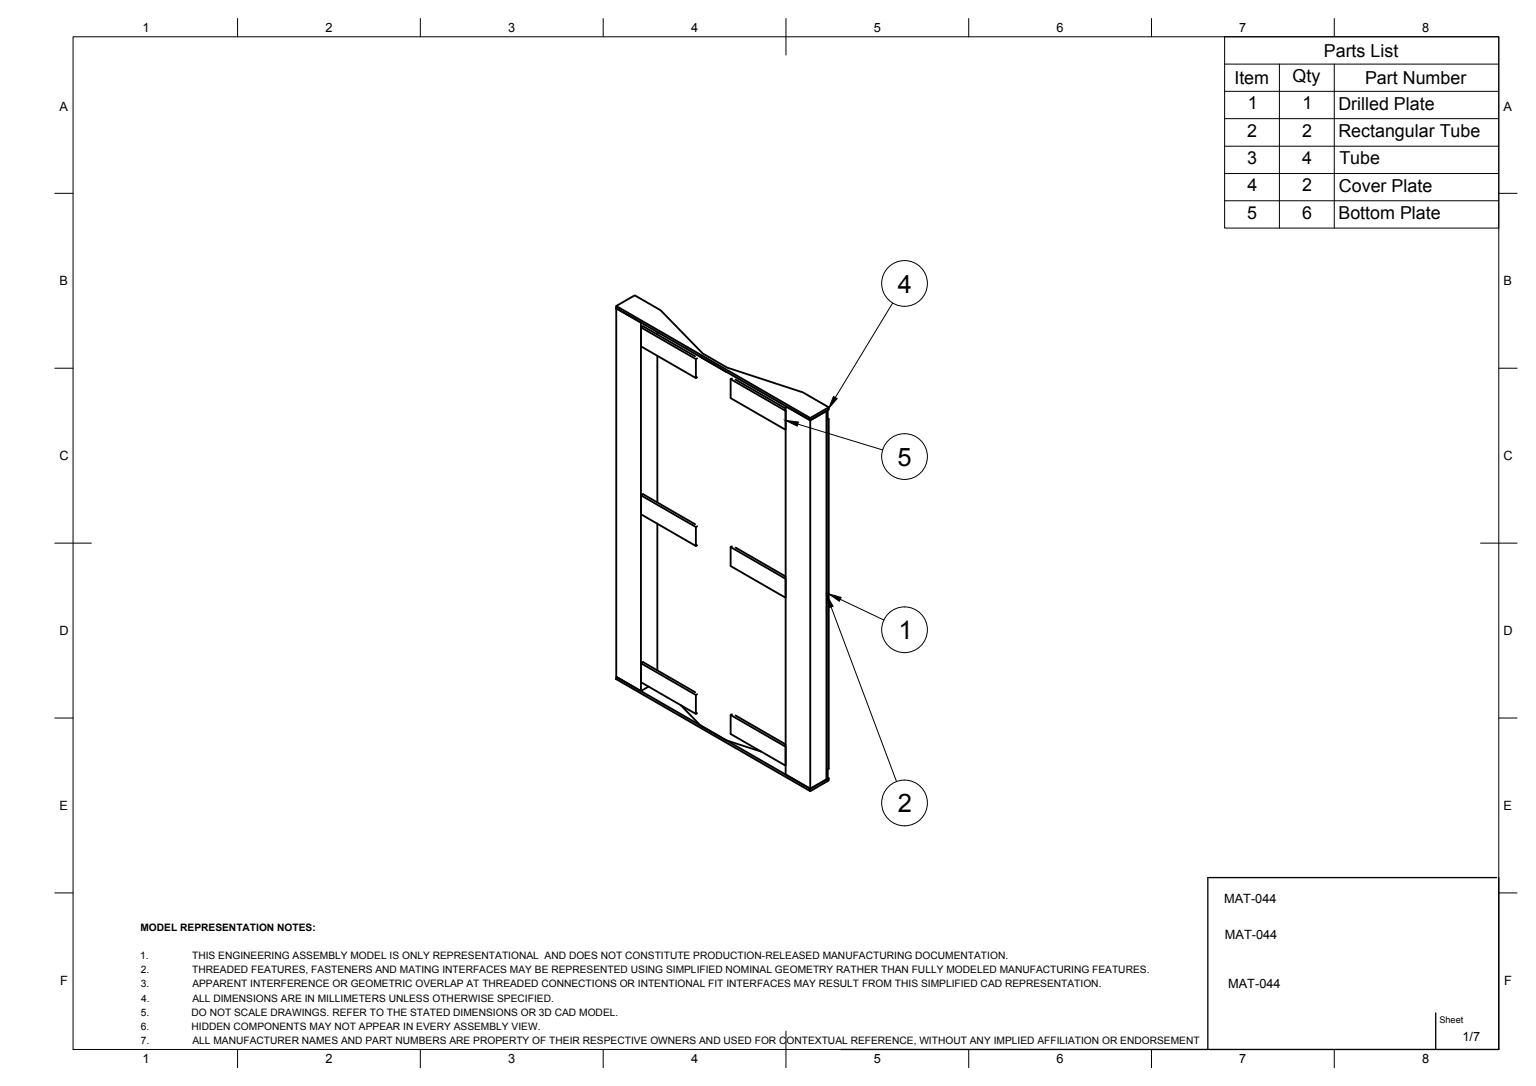
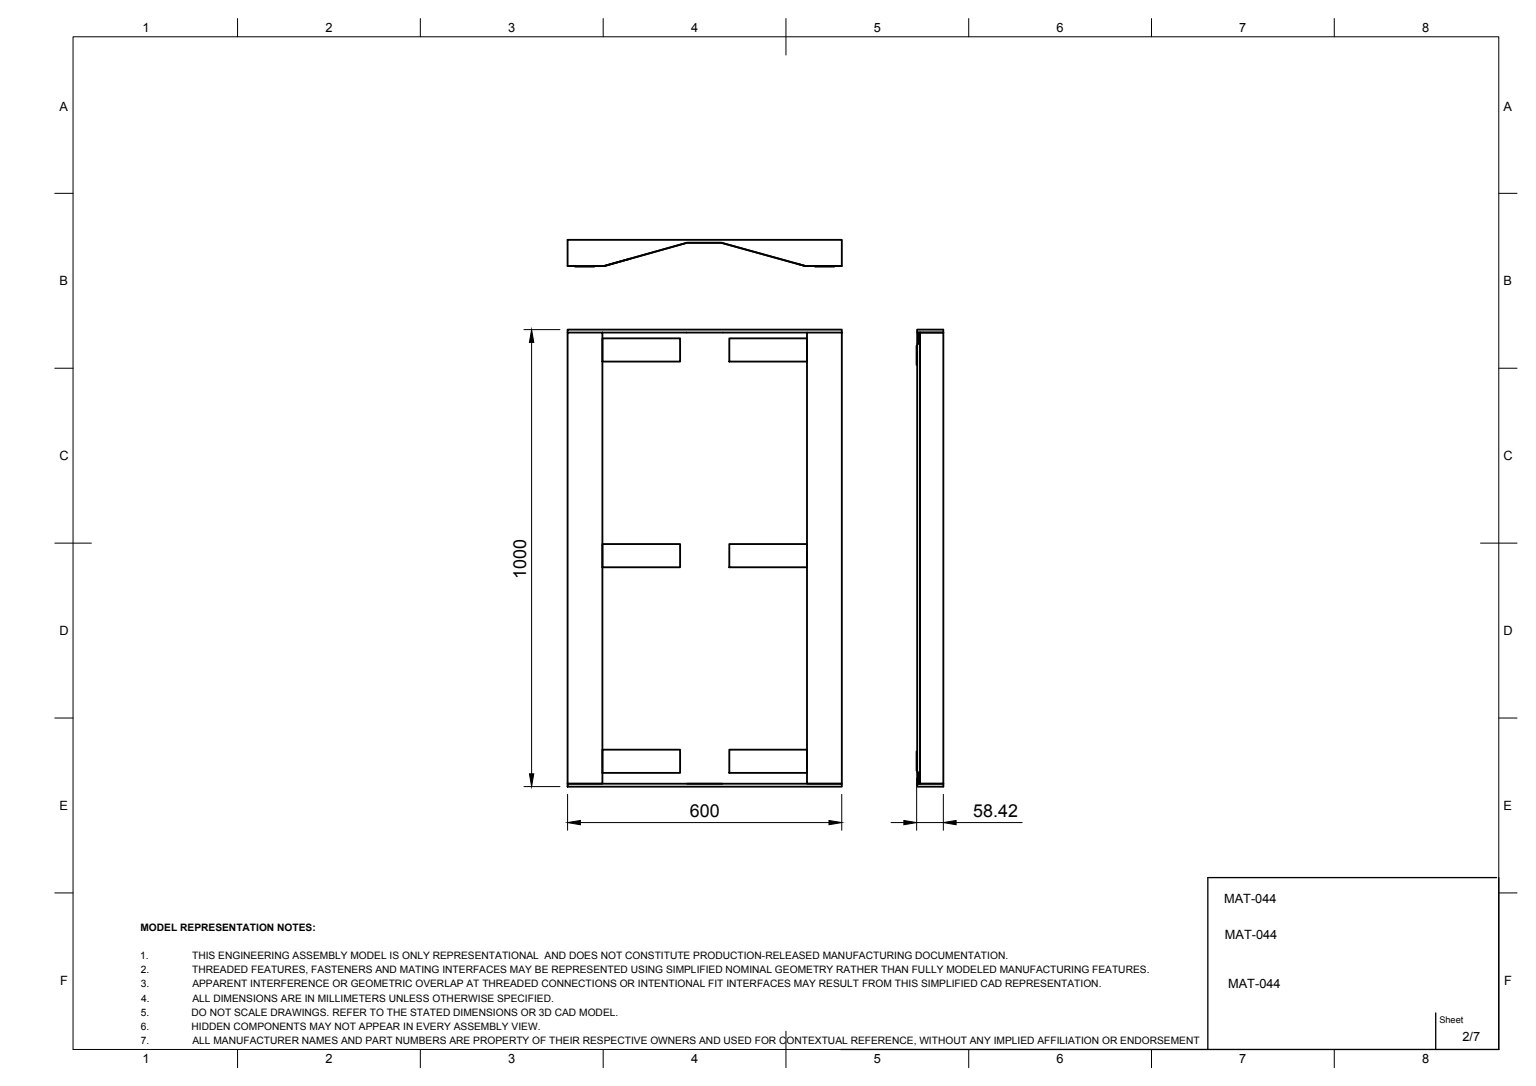
ISO-10303-21;
HEADER;
/* Generated by software containing ST-Developer
 * from STEP Tools, Inc. (www.steptools.com) 
 */

FILE_DESCRIPTION(
/* description */ ('STEP AP214'),
/* implementation_level */ '2;1');

FILE_NAME(
/* name */ 'MAT-044.step',
/* time_stamp */ '2026-11-14T22:20:24-08:00',
/* author */ (''),
/* organization */ (''),
/* preprocessor_version */ 'ST-DEVELOPER v20.2',
/* originating_system */ 'Autodesk Translation Framework v15.17.0.0',
/* authorisation */ '');

FILE_SCHEMA (('AUTOMOTIVE_DESIGN { 1 0 10303 214 3 1 1 }'));
ENDSEC;

DATA;
#10=MECHANICAL_DESIGN_GEOMETRIC_PRESENTATION_REPRESENTATION('',(#82,#83,
#84,#85,#86),#2794);
#11=ITEM_DEFINED_TRANSFORMATION($,$,#1703,#1840);
#12=ITEM_DEFINED_TRANSFORMATION($,$,#1794,#1841);
#13=ITEM_DEFINED_TRANSFORMATION($,$,#1829,#1842);
#14=ITEM_DEFINED_TRANSFORMATION($,$,#1811,#1843);
#15=ITEM_DEFINED_TRANSFORMATION($,$,#1822,#1844);
#16=ITEM_DEFINED_TRANSFORMATION($,$,#1794,#1845);
#17=ITEM_DEFINED_TRANSFORMATION($,$,#1811,#1846);
#18=ITEM_DEFINED_TRANSFORMATION($,$,#1822,#1847);
#19=ITEM_DEFINED_TRANSFORMATION($,$,#1822,#1848);
#20=ITEM_DEFINED_TRANSFORMATION($,$,#1822,#1849);
#21=ITEM_DEFINED_TRANSFORMATION($,$,#1822,#1850);
#22=ITEM_DEFINED_TRANSFORMATION($,$,#1822,#1851);
#23=ITEM_DEFINED_TRANSFORMATION($,$,#1829,#1852);
#24=ITEM_DEFINED_TRANSFORMATION($,$,#1829,#1853);
#25=ITEM_DEFINED_TRANSFORMATION($,$,#1829,#1854);
#26=(
REPRESENTATION_RELATIONSHIP($,$,#2827,#2826)
REPRESENTATION_RELATIONSHIP_WITH_TRANSFORMATION(#11)
SHAPE_REPRESENTATION_RELATIONSHIP()
);
#27=(
REPRESENTATION_RELATIONSHIP($,$,#2828,#2826)
REPRESENTATION_RELATIONSHIP_WITH_TRANSFORMATION(#12)
SHAPE_REPRESENTATION_RELATIONSHIP()
);
#28=(
REPRESENTATION_RELATIONSHIP($,$,#2831,#2826)
REPRESENTATION_RELATIONSHIP_WITH_TRANSFORMATION(#13)
SHAPE_REPRESENTATION_RELATIONSHIP()
);
#29=(
REPRESENTATION_RELATIONSHIP($,$,#2829,#2826)
REPRESENTATION_RELATIONSHIP_WITH_TRANSFORMATION(#14)
SHAPE_REPRESENTATION_RELATIONSHIP()
);
#30=(
REPRESENTATION_RELATIONSHIP($,$,#2830,#2826)
REPRESENTATION_RELATIONSHIP_WITH_TRANSFORMATION(#15)
SHAPE_REPRESENTATION_RELATIONSHIP()
);
#31=(
REPRESENTATION_RELATIONSHIP($,$,#2828,#2826)
REPRESENTATION_RELATIONSHIP_WITH_TRANSFORMATION(#16)
SHAPE_REPRESENTATION_RELATIONSHIP()
);
#32=(
REPRESENTATION_RELATIONSHIP($,$,#2829,#2826)
REPRESENTATION_RELATIONSHIP_WITH_TRANSFORMATION(#17)
SHAPE_REPRESENTATION_RELATIONSHIP()
);
#33=(
REPRESENTATION_RELATIONSHIP($,$,#2830,#2826)
REPRESENTATION_RELATIONSHIP_WITH_TRANSFORMATION(#18)
SHAPE_REPRESENTATION_RELATIONSHIP()
);
#34=(
REPRESENTATION_RELATIONSHIP($,$,#2830,#2826)
REPRESENTATION_RELATIONSHIP_WITH_TRANSFORMATION(#19)
SHAPE_REPRESENTATION_RELATIONSHIP()
);
#35=(
REPRESENTATION_RELATIONSHIP($,$,#2830,#2826)
REPRESENTATION_RELATIONSHIP_WITH_TRANSFORMATION(#20)
SHAPE_REPRESENTATION_RELATIONSHIP()
);
#36=(
REPRESENTATION_RELATIONSHIP($,$,#2830,#2826)
REPRESENTATION_RELATIONSHIP_WITH_TRANSFORMATION(#21)
SHAPE_REPRESENTATION_RELATIONSHIP()
);
#37=(
REPRESENTATION_RELATIONSHIP($,$,#2830,#2826)
REPRESENTATION_RELATIONSHIP_WITH_TRANSFORMATION(#22)
SHAPE_REPRESENTATION_RELATIONSHIP()
);
#38=(
REPRESENTATION_RELATIONSHIP($,$,#2831,#2826)
REPRESENTATION_RELATIONSHIP_WITH_TRANSFORMATION(#23)
SHAPE_REPRESENTATION_RELATIONSHIP()
);
#39=(
REPRESENTATION_RELATIONSHIP($,$,#2831,#2826)
REPRESENTATION_RELATIONSHIP_WITH_TRANSFORMATION(#24)
SHAPE_REPRESENTATION_RELATIONSHIP()
);
#40=(
REPRESENTATION_RELATIONSHIP($,$,#2831,#2826)
REPRESENTATION_RELATIONSHIP_WITH_TRANSFORMATION(#25)
SHAPE_REPRESENTATION_RELATIONSHIP()
);
#41=CONTEXT_DEPENDENT_SHAPE_REPRESENTATION(#26,#2811);
#42=CONTEXT_DEPENDENT_SHAPE_REPRESENTATION(#27,#2812);
#43=CONTEXT_DEPENDENT_SHAPE_REPRESENTATION(#28,#2813);
#44=CONTEXT_DEPENDENT_SHAPE_REPRESENTATION(#29,#2814);
#45=CONTEXT_DEPENDENT_SHAPE_REPRESENTATION(#30,#2815);
#46=CONTEXT_DEPENDENT_SHAPE_REPRESENTATION(#31,#2816);
#47=CONTEXT_DEPENDENT_SHAPE_REPRESENTATION(#32,#2817);
#48=CONTEXT_DEPENDENT_SHAPE_REPRESENTATION(#33,#2818);
#49=CONTEXT_DEPENDENT_SHAPE_REPRESENTATION(#34,#2819);
#50=CONTEXT_DEPENDENT_SHAPE_REPRESENTATION(#35,#2820);
#51=CONTEXT_DEPENDENT_SHAPE_REPRESENTATION(#36,#2821);
#52=CONTEXT_DEPENDENT_SHAPE_REPRESENTATION(#37,#2822);
#53=CONTEXT_DEPENDENT_SHAPE_REPRESENTATION(#38,#2823);
#54=CONTEXT_DEPENDENT_SHAPE_REPRESENTATION(#39,#2824);
#55=CONTEXT_DEPENDENT_SHAPE_REPRESENTATION(#40,#2825);
#56=NEXT_ASSEMBLY_USAGE_OCCURRENCE('Drilled Plate:1','Drilled Plate:1',
'Drilled Plate:1',#2833,#2834,'Drilled Plate:1');
#57=NEXT_ASSEMBLY_USAGE_OCCURRENCE('Rectangular Tube:1',
'Rectangular Tube:1','Rectangular Tube:1',#2833,#2835,
'Rectangular Tube:1');
#58=NEXT_ASSEMBLY_USAGE_OCCURRENCE('Tube:1','Tube:1','Tube:1',#2833,#2838,
'Tube:1');
#59=NEXT_ASSEMBLY_USAGE_OCCURRENCE('Cover Plate:1','Cover Plate:1',
'Cover Plate:1',#2833,#2836,'Cover Plate:1');
#60=NEXT_ASSEMBLY_USAGE_OCCURRENCE('Bottom Plate:1','Bottom Plate:1',
'Bottom Plate:1',#2833,#2837,'Bottom Plate:1');
#61=NEXT_ASSEMBLY_USAGE_OCCURRENCE('Rectangular Tube:2',
'Rectangular Tube:2','Rectangular Tube:2',#2833,#2835,
'Rectangular Tube:2');
#62=NEXT_ASSEMBLY_USAGE_OCCURRENCE('Cover Plate:2','Cover Plate:2',
'Cover Plate:2',#2833,#2836,'Cover Plate:2');
#63=NEXT_ASSEMBLY_USAGE_OCCURRENCE('Bottom Plate:2','Bottom Plate:2',
'Bottom Plate:2',#2833,#2837,'Bottom Plate:2');
#64=NEXT_ASSEMBLY_USAGE_OCCURRENCE('Bottom Plate:3','Bottom Plate:3',
'Bottom Plate:3',#2833,#2837,'Bottom Plate:3');
#65=NEXT_ASSEMBLY_USAGE_OCCURRENCE('Bottom Plate:4','Bottom Plate:4',
'Bottom Plate:4',#2833,#2837,'Bottom Plate:4');
#66=NEXT_ASSEMBLY_USAGE_OCCURRENCE('Bottom Plate:5','Bottom Plate:5',
'Bottom Plate:5',#2833,#2837,'Bottom Plate:5');
#67=NEXT_ASSEMBLY_USAGE_OCCURRENCE('Bottom Plate:6','Bottom Plate:6',
'Bottom Plate:6',#2833,#2837,'Bottom Plate:6');
#68=NEXT_ASSEMBLY_USAGE_OCCURRENCE('Tube:2','Tube:2','Tube:2',#2833,#2838,
'Tube:2');
#69=NEXT_ASSEMBLY_USAGE_OCCURRENCE('Tube:3','Tube:3','Tube:3',#2833,#2838,
'Tube:3');
#70=NEXT_ASSEMBLY_USAGE_OCCURRENCE('Tube:4','Tube:4','Tube:4',#2833,#2838,
'Tube:4');
#71=CONICAL_SURFACE('',#1830,18.6799999999998,0.785398163397447);
#72=SHAPE_REPRESENTATION_RELATIONSHIP('SRR','None',#2827,#77);
#73=SHAPE_REPRESENTATION_RELATIONSHIP('SRR','None',#2828,#78);
#74=SHAPE_REPRESENTATION_RELATIONSHIP('SRR','None',#2829,#79);
#75=SHAPE_REPRESENTATION_RELATIONSHIP('SRR','None',#2830,#80);
#76=SHAPE_REPRESENTATION_RELATIONSHIP('SRR','None',#2831,#81);
#77=ADVANCED_BREP_SHAPE_REPRESENTATION('',(#87),#2789);
#78=ADVANCED_BREP_SHAPE_REPRESENTATION('',(#88),#2790);
#79=ADVANCED_BREP_SHAPE_REPRESENTATION('',(#89),#2791);
#80=ADVANCED_BREP_SHAPE_REPRESENTATION('',(#90),#2792);
#81=ADVANCED_BREP_SHAPE_REPRESENTATION('',(#91),#2793);
#82=STYLED_ITEM('',(#2861),#87);
#83=STYLED_ITEM('',(#2862),#88);
#84=STYLED_ITEM('',(#2863),#89);
#85=STYLED_ITEM('',(#2863),#90);
#86=STYLED_ITEM('',(#2863),#91);
#87=MANIFOLD_SOLID_BREP('Body1',#1641);
#88=MANIFOLD_SOLID_BREP('Body1',#1642);
#89=MANIFOLD_SOLID_BREP('Body1',#1643);
#90=MANIFOLD_SOLID_BREP('Body1',#1644);
#91=MANIFOLD_SOLID_BREP('Body1',#1645);
#92=FACE_BOUND('',#286,.T.);
#93=FACE_BOUND('',#287,.T.);
#94=FACE_BOUND('',#288,.T.);
#95=FACE_BOUND('',#289,.T.);
#96=FACE_BOUND('',#291,.T.);
#97=FACE_BOUND('',#292,.T.);
#98=FACE_BOUND('',#293,.T.);
#99=FACE_BOUND('',#294,.T.);
#100=FACE_BOUND('',#296,.T.);
#101=FACE_BOUND('',#297,.T.);
#102=FACE_BOUND('',#299,.T.);
#103=FACE_BOUND('',#300,.T.);
#104=FACE_BOUND('',#338,.T.);
#105=FACE_BOUND('',#342,.T.);
#106=FACE_BOUND('',#346,.T.);
#107=FACE_BOUND('',#350,.T.);
#108=FACE_BOUND('',#354,.T.);
#109=FACE_BOUND('',#355,.T.);
#110=FACE_BOUND('',#362,.T.);
#111=FACE_BOUND('',#363,.T.);
#112=FACE_BOUND('',#366,.T.);
#113=FACE_BOUND('',#368,.T.);
#114=FACE_BOUND('',#389,.T.);
#115=FACE_BOUND('',#391,.T.);
#116=PLANE('',#1728);
#117=PLANE('',#1729);
#118=PLANE('',#1730);
#119=PLANE('',#1731);
#120=PLANE('',#1732);
#121=PLANE('',#1733);
#122=PLANE('',#1734);
#123=PLANE('',#1735);
#124=PLANE('',#1736);
#125=PLANE('',#1739);
#126=PLANE('',#1740);
#127=PLANE('',#1743);
#128=PLANE('',#1746);
#129=PLANE('',#1747);
#130=PLANE('',#1750);
#131=PLANE('',#1751);
#132=PLANE('',#1754);
#133=PLANE('',#1755);
#134=PLANE('',#1758);
#135=PLANE('',#1759);
#136=PLANE('',#1762);
#137=PLANE('',#1765);
#138=PLANE('',#1767);
#139=PLANE('',#1769);
#140=PLANE('',#1771);
#141=PLANE('',#1774);
#142=PLANE('',#1776);
#143=PLANE('',#1778);
#144=PLANE('',#1780);
#145=PLANE('',#1781);
#146=PLANE('',#1782);
#147=PLANE('',#1783);
#148=PLANE('',#1784);
#149=PLANE('',#1785);
#150=PLANE('',#1786);
#151=PLANE('',#1787);
#152=PLANE('',#1788);
#153=PLANE('',#1789);
#154=PLANE('',#1790);
#155=PLANE('',#1791);
#156=PLANE('',#1792);
#157=PLANE('',#1793);
#158=PLANE('',#1801);
#159=PLANE('',#1802);
#160=PLANE('',#1803);
#161=PLANE('',#1804);
#162=PLANE('',#1805);
#163=PLANE('',#1806);
#164=PLANE('',#1807);
#165=PLANE('',#1808);
#166=PLANE('',#1809);
#167=PLANE('',#1810);
#168=PLANE('',#1812);
#169=PLANE('',#1813);
#170=PLANE('',#1814);
#171=PLANE('',#1815);
#172=PLANE('',#1816);
#173=PLANE('',#1817);
#174=PLANE('',#1818);
#175=PLANE('',#1819);
#176=PLANE('',#1820);
#177=PLANE('',#1821);
#178=PLANE('',#1823);
#179=PLANE('',#1824);
#180=PLANE('',#1825);
#181=PLANE('',#1826);
#182=PLANE('',#1827);
#183=PLANE('',#1828);
#184=PLANE('',#1838);
#185=PLANE('',#1839);
#186=FACE_OUTER_BOUND('',#277,.T.);
#187=FACE_OUTER_BOUND('',#278,.T.);
#188=FACE_OUTER_BOUND('',#279,.T.);
#189=FACE_OUTER_BOUND('',#280,.T.);
#190=FACE_OUTER_BOUND('',#281,.T.);
#191=FACE_OUTER_BOUND('',#282,.T.);
#192=FACE_OUTER_BOUND('',#283,.T.);
#193=FACE_OUTER_BOUND('',#284,.T.);
#194=FACE_OUTER_BOUND('',#285,.T.);
#195=FACE_OUTER_BOUND('',#290,.T.);
#196=FACE_OUTER_BOUND('',#295,.T.);
#197=FACE_OUTER_BOUND('',#298,.T.);
#198=FACE_OUTER_BOUND('',#301,.T.);
#199=FACE_OUTER_BOUND('',#302,.T.);
#200=FACE_OUTER_BOUND('',#303,.T.);
#201=FACE_OUTER_BOUND('',#304,.T.);
#202=FACE_OUTER_BOUND('',#305,.T.);
#203=FACE_OUTER_BOUND('',#306,.T.);
#204=FACE_OUTER_BOUND('',#307,.T.);
#205=FACE_OUTER_BOUND('',#308,.T.);
#206=FACE_OUTER_BOUND('',#309,.T.);
#207=FACE_OUTER_BOUND('',#310,.T.);
#208=FACE_OUTER_BOUND('',#311,.T.);
#209=FACE_OUTER_BOUND('',#312,.T.);
#210=FACE_OUTER_BOUND('',#313,.T.);
#211=FACE_OUTER_BOUND('',#314,.T.);
#212=FACE_OUTER_BOUND('',#315,.T.);
#213=FACE_OUTER_BOUND('',#316,.T.);
#214=FACE_OUTER_BOUND('',#317,.T.);
#215=FACE_OUTER_BOUND('',#318,.T.);
#216=FACE_OUTER_BOUND('',#319,.T.);
#217=FACE_OUTER_BOUND('',#320,.T.);
#218=FACE_OUTER_BOUND('',#321,.T.);
#219=FACE_OUTER_BOUND('',#322,.T.);
#220=FACE_OUTER_BOUND('',#323,.T.);
#221=FACE_OUTER_BOUND('',#324,.T.);
#222=FACE_OUTER_BOUND('',#325,.T.);
#223=FACE_OUTER_BOUND('',#326,.T.);
#224=FACE_OUTER_BOUND('',#327,.T.);
#225=FACE_OUTER_BOUND('',#328,.T.);
#226=FACE_OUTER_BOUND('',#329,.T.);
#227=FACE_OUTER_BOUND('',#330,.T.);
#228=FACE_OUTER_BOUND('',#331,.T.);
#229=FACE_OUTER_BOUND('',#332,.T.);
#230=FACE_OUTER_BOUND('',#333,.T.);
#231=FACE_OUTER_BOUND('',#334,.T.);
#232=FACE_OUTER_BOUND('',#335,.T.);
#233=FACE_OUTER_BOUND('',#336,.T.);
#234=FACE_OUTER_BOUND('',#337,.T.);
#235=FACE_OUTER_BOUND('',#339,.T.);
#236=FACE_OUTER_BOUND('',#340,.T.);
#237=FACE_OUTER_BOUND('',#341,.T.);
#238=FACE_OUTER_BOUND('',#343,.T.);
#239=FACE_OUTER_BOUND('',#344,.T.);
#240=FACE_OUTER_BOUND('',#345,.T.);
#241=FACE_OUTER_BOUND('',#347,.T.);
#242=FACE_OUTER_BOUND('',#348,.T.);
#243=FACE_OUTER_BOUND('',#349,.T.);
#244=FACE_OUTER_BOUND('',#351,.T.);
#245=FACE_OUTER_BOUND('',#352,.T.);
#246=FACE_OUTER_BOUND('',#353,.T.);
#247=FACE_OUTER_BOUND('',#356,.T.);
#248=FACE_OUTER_BOUND('',#357,.T.);
#249=FACE_OUTER_BOUND('',#358,.T.);
#250=FACE_OUTER_BOUND('',#359,.T.);
#251=FACE_OUTER_BOUND('',#360,.T.);
#252=FACE_OUTER_BOUND('',#361,.T.);
#253=FACE_OUTER_BOUND('',#364,.T.);
#254=FACE_OUTER_BOUND('',#365,.T.);
#255=FACE_OUTER_BOUND('',#367,.T.);
#256=FACE_OUTER_BOUND('',#369,.T.);
#257=FACE_OUTER_BOUND('',#370,.T.);
#258=FACE_OUTER_BOUND('',#371,.T.);
#259=FACE_OUTER_BOUND('',#372,.T.);
#260=FACE_OUTER_BOUND('',#373,.T.);
#261=FACE_OUTER_BOUND('',#374,.T.);
#262=FACE_OUTER_BOUND('',#375,.T.);
#263=FACE_OUTER_BOUND('',#376,.T.);
#264=FACE_OUTER_BOUND('',#377,.T.);
#265=FACE_OUTER_BOUND('',#378,.T.);
#266=FACE_OUTER_BOUND('',#379,.T.);
#267=FACE_OUTER_BOUND('',#380,.T.);
#268=FACE_OUTER_BOUND('',#381,.T.);
#269=FACE_OUTER_BOUND('',#382,.T.);
#270=FACE_OUTER_BOUND('',#383,.T.);
#271=FACE_OUTER_BOUND('',#384,.T.);
#272=FACE_OUTER_BOUND('',#385,.T.);
#273=FACE_OUTER_BOUND('',#386,.T.);
#274=FACE_OUTER_BOUND('',#387,.T.);
#275=FACE_OUTER_BOUND('',#388,.T.);
#276=FACE_OUTER_BOUND('',#390,.T.);
#277=EDGE_LOOP('',(#1110,#1111,#1112,#1113));
#278=EDGE_LOOP('',(#1114,#1115,#1116,#1117));
#279=EDGE_LOOP('',(#1118,#1119,#1120,#1121));
#280=EDGE_LOOP('',(#1122,#1123,#1124,#1125));
#281=EDGE_LOOP('',(#1126,#1127,#1128,#1129));
#282=EDGE_LOOP('',(#1130,#1131,#1132,#1133));
#283=EDGE_LOOP('',(#1134,#1135,#1136,#1137));
#284=EDGE_LOOP('',(#1138,#1139,#1140,#1141));
#285=EDGE_LOOP('',(#1142,#1143,#1144,#1145));
#286=EDGE_LOOP('',(#1146));
#287=EDGE_LOOP('',(#1147));
#288=EDGE_LOOP('',(#1148));
#289=EDGE_LOOP('',(#1149));
#290=EDGE_LOOP('',(#1150,#1151,#1152,#1153));
#291=EDGE_LOOP('',(#1154));
#292=EDGE_LOOP('',(#1155));
#293=EDGE_LOOP('',(#1156));
#294=EDGE_LOOP('',(#1157));
#295=EDGE_LOOP('',(#1158,#1159,#1160,#1161,#1162,#1163,#1164,#1165));
#296=EDGE_LOOP('',(#1166));
#297=EDGE_LOOP('',(#1167));
#298=EDGE_LOOP('',(#1168,#1169,#1170,#1171,#1172,#1173,#1174,#1175));
#299=EDGE_LOOP('',(#1176));
#300=EDGE_LOOP('',(#1177));
#301=EDGE_LOOP('',(#1178,#1179,#1180,#1181,#1182,#1183));
#302=EDGE_LOOP('',(#1184,#1185,#1186,#1187,#1188,#1189));
#303=EDGE_LOOP('',(#1190,#1191,#1192,#1193,#1194,#1195,#1196,#1197));
#304=EDGE_LOOP('',(#1198,#1199,#1200,#1201,#1202,#1203,#1204,#1205));
#305=EDGE_LOOP('',(#1206,#1207,#1208,#1209));
#306=EDGE_LOOP('',(#1210,#1211,#1212,#1213));
#307=EDGE_LOOP('',(#1214,#1215,#1216,#1217));
#308=EDGE_LOOP('',(#1218,#1219,#1220,#1221));
#309=EDGE_LOOP('',(#1222,#1223,#1224,#1225));
#310=EDGE_LOOP('',(#1226,#1227,#1228,#1229));
#311=EDGE_LOOP('',(#1230,#1231,#1232,#1233));
#312=EDGE_LOOP('',(#1234,#1235,#1236,#1237));
#313=EDGE_LOOP('',(#1238,#1239,#1240,#1241));
#314=EDGE_LOOP('',(#1242,#1243,#1244,#1245));
#315=EDGE_LOOP('',(#1246,#1247,#1248,#1249));
#316=EDGE_LOOP('',(#1250,#1251,#1252,#1253));
#317=EDGE_LOOP('',(#1254,#1255,#1256,#1257));
#318=EDGE_LOOP('',(#1258,#1259,#1260,#1261));
#319=EDGE_LOOP('',(#1262,#1263,#1264,#1265));
#320=EDGE_LOOP('',(#1266,#1267,#1268,#1269));
#321=EDGE_LOOP('',(#1270,#1271,#1272,#1273));
#322=EDGE_LOOP('',(#1274,#1275,#1276,#1277));
#323=EDGE_LOOP('',(#1278,#1279,#1280,#1281));
#324=EDGE_LOOP('',(#1282,#1283,#1284,#1285));
#325=EDGE_LOOP('',(#1286,#1287,#1288,#1289));
#326=EDGE_LOOP('',(#1290,#1291,#1292,#1293));
#327=EDGE_LOOP('',(#1294,#1295,#1296,#1297));
#328=EDGE_LOOP('',(#1298,#1299,#1300,#1301));
#329=EDGE_LOOP('',(#1302,#1303,#1304,#1305));
#330=EDGE_LOOP('',(#1306,#1307,#1308,#1309));
#331=EDGE_LOOP('',(#1310,#1311,#1312,#1313));
#332=EDGE_LOOP('',(#1314,#1315,#1316,#1317));
#333=EDGE_LOOP('',(#1318,#1319,#1320,#1321,#1322,#1323));
#334=EDGE_LOOP('',(#1324,#1325,#1326,#1327,#1328,#1329));
#335=EDGE_LOOP('',(#1330,#1331,#1332,#1333));
#336=EDGE_LOOP('',(#1334,#1335,#1336,#1337));
#337=EDGE_LOOP('',(#1338,#1339,#1340,#1341));
#338=EDGE_LOOP('',(#1342));
#339=EDGE_LOOP('',(#1343,#1344,#1345,#1346));
#340=EDGE_LOOP('',(#1347,#1348,#1349,#1350));
#341=EDGE_LOOP('',(#1351,#1352,#1353,#1354));
#342=EDGE_LOOP('',(#1355));
#343=EDGE_LOOP('',(#1356,#1357,#1358,#1359));
#344=EDGE_LOOP('',(#1360,#1361,#1362,#1363));
#345=EDGE_LOOP('',(#1364,#1365,#1366,#1367));
#346=EDGE_LOOP('',(#1368));
#347=EDGE_LOOP('',(#1369,#1370,#1371,#1372));
#348=EDGE_LOOP('',(#1373,#1374,#1375,#1376));
#349=EDGE_LOOP('',(#1377,#1378,#1379,#1380));
#350=EDGE_LOOP('',(#1381));
#351=EDGE_LOOP('',(#1382,#1383,#1384,#1385));
#352=EDGE_LOOP('',(#1386,#1387,#1388,#1389));
#353=EDGE_LOOP('',(#1390,#1391,#1392,#1393));
#354=EDGE_LOOP('',(#1394));
#355=EDGE_LOOP('',(#1395));
#356=EDGE_LOOP('',(#1396,#1397,#1398,#1399));
#357=EDGE_LOOP('',(#1400,#1401,#1402,#1403));
#358=EDGE_LOOP('',(#1404,#1405,#1406,#1407));
#359=EDGE_LOOP('',(#1408,#1409,#1410,#1411));
#360=EDGE_LOOP('',(#1412,#1413,#1414,#1415));
#361=EDGE_LOOP('',(#1416,#1417,#1418,#1419));
#362=EDGE_LOOP('',(#1420));
#363=EDGE_LOOP('',(#1421));
#364=EDGE_LOOP('',(#1422,#1423,#1424,#1425));
#365=EDGE_LOOP('',(#1426,#1427,#1428,#1429));
#366=EDGE_LOOP('',(#1430,#1431,#1432,#1433));
#367=EDGE_LOOP('',(#1434,#1435,#1436,#1437));
#368=EDGE_LOOP('',(#1438,#1439,#1440,#1441));
#369=EDGE_LOOP('',(#1442,#1443,#1444,#1445));
#370=EDGE_LOOP('',(#1446,#1447,#1448,#1449));
#371=EDGE_LOOP('',(#1450,#1451,#1452,#1453));
#372=EDGE_LOOP('',(#1454,#1455,#1456,#1457));
#373=EDGE_LOOP('',(#1458,#1459,#1460,#1461));
#374=EDGE_LOOP('',(#1462,#1463,#1464,#1465));
#375=EDGE_LOOP('',(#1466,#1467,#1468,#1469));
#376=EDGE_LOOP('',(#1470,#1471,#1472,#1473));
#377=EDGE_LOOP('',(#1474,#1475,#1476,#1477,#1478,#1479,#1480,#1481));
#378=EDGE_LOOP('',(#1482,#1483,#1484,#1485,#1486,#1487,#1488,#1489));
#379=EDGE_LOOP('',(#1490,#1491,#1492,#1493));
#380=EDGE_LOOP('',(#1494,#1495,#1496,#1497));
#381=EDGE_LOOP('',(#1498,#1499,#1500,#1501));
#382=EDGE_LOOP('',(#1502,#1503,#1504,#1505));
#383=EDGE_LOOP('',(#1506,#1507,#1508,#1509));
#384=EDGE_LOOP('',(#1510,#1511,#1512,#1513));
#385=EDGE_LOOP('',(#1514,#1515,#1516,#1517));
#386=EDGE_LOOP('',(#1518,#1519,#1520,#1521));
#387=EDGE_LOOP('',(#1522,#1523,#1524,#1525));
#388=EDGE_LOOP('',(#1526));
#389=EDGE_LOOP('',(#1527));
#390=EDGE_LOOP('',(#1528));
#391=EDGE_LOOP('',(#1529));
#392=LINE('',#2336,#561);
#393=LINE('',#2342,#562);
#394=LINE('',#2348,#563);
#395=LINE('',#2354,#564);
#396=LINE('',#2360,#565);
#397=LINE('',#2366,#566);
#398=LINE('',#2372,#567);
#399=LINE('',#2378,#568);
#400=LINE('',#2383,#569);
#401=LINE('',#2385,#570);
#402=LINE('',#2387,#571);
#403=LINE('',#2388,#572);
#404=LINE('',#2392,#573);
#405=LINE('',#2394,#574);
#406=LINE('',#2396,#575);
#407=LINE('',#2397,#576);
#408=LINE('',#2401,#577);
#409=LINE('',#2403,#578);
#410=LINE('',#2405,#579);
#411=LINE('',#2407,#580);
#412=LINE('',#2409,#581);
#413=LINE('',#2411,#582);
#414=LINE('',#2413,#583);
#415=LINE('',#2414,#584);
#416=LINE('',#2418,#585);
#417=LINE('',#2420,#586);
#418=LINE('',#2422,#587);
#419=LINE('',#2424,#588);
#420=LINE('',#2426,#589);
#421=LINE('',#2428,#590);
#422=LINE('',#2430,#591);
#423=LINE('',#2431,#592);
#424=LINE('',#2435,#593);
#425=LINE('',#2436,#594);
#426=LINE('',#2437,#595);
#427=LINE('',#2438,#596);
#428=LINE('',#2442,#597);
#429=LINE('',#2443,#598);
#430=LINE('',#2444,#599);
#431=LINE('',#2445,#600);
#432=LINE('',#2448,#601);
#433=LINE('',#2449,#602);
#434=LINE('',#2451,#603);
#435=LINE('',#2453,#604);
#436=LINE('',#2454,#605);
#437=LINE('',#2458,#606);
#438=LINE('',#2459,#607);
#439=LINE('',#2461,#608);
#440=LINE('',#2462,#609);
#441=LINE('',#2463,#610);
#442=LINE('',#2467,#611);
#443=LINE('',#2469,#612);
#444=LINE('',#2473,#613);
#445=LINE('',#2475,#614);
#446=LINE('',#2476,#615);
#447=LINE('',#2481,#616);
#448=LINE('',#2486,#617);
#449=LINE('',#2491,#618);
#450=LINE('',#2493,#619);
#451=LINE('',#2494,#620);
#452=LINE('',#2498,#621);
#453=LINE('',#2502,#622);
#454=LINE('',#2505,#623);
#455=LINE('',#2506,#624);
#456=LINE('',#2510,#625);
#457=LINE('',#2515,#626);
#458=LINE('',#2517,#627);
#459=LINE('',#2518,#628);
#460=LINE('',#2522,#629);
#461=LINE('',#2526,#630);
#462=LINE('',#2529,#631);
#463=LINE('',#2530,#632);
#464=LINE('',#2537,#633);
#465=LINE('',#2539,#634);
#466=LINE('',#2542,#635);
#467=LINE('',#2543,#636);
#468=LINE('',#2545,#637);
#469=LINE('',#2547,#638);
#470=LINE('',#2549,#639);
#471=LINE('',#2551,#640);
#472=LINE('',#2553,#641);
#473=LINE('',#2555,#642);
#474=LINE('',#2558,#643);
#475=LINE('',#2560,#644);
#476=LINE('',#2562,#645);
#477=LINE('',#2564,#646);
#478=LINE('',#2566,#647);
#479=LINE('',#2568,#648);
#480=LINE('',#2572,#649);
#481=LINE('',#2573,#650);
#482=LINE('',#2576,#651);
#483=LINE('',#2577,#652);
#484=LINE('',#2580,#653);
#485=LINE('',#2581,#654);
#486=LINE('',#2583,#655);
#487=LINE('',#2587,#656);
#488=LINE('',#2588,#657);
#489=LINE('',#2590,#658);
#490=LINE('',#2594,#659);
#491=LINE('',#2595,#660);
#492=LINE('',#2597,#661);
#493=LINE('',#2601,#662);
#494=LINE('',#2602,#663);
#495=LINE('',#2604,#664);
#496=LINE('',#2611,#665);
#497=LINE('',#2617,#666);
#498=LINE('',#2622,#667);
#499=LINE('',#2624,#668);
#500=LINE('',#2626,#669);
#501=LINE('',#2627,#670);
#502=LINE('',#2630,#671);
#503=LINE('',#2632,#672);
#504=LINE('',#2633,#673);
#505=LINE('',#2636,#674);
#506=LINE('',#2638,#675);
#507=LINE('',#2639,#676);
#508=LINE('',#2643,#677);
#509=LINE('',#2645,#678);
#510=LINE('',#2647,#679);
#511=LINE('',#2648,#680);
#512=LINE('',#2651,#681);
#513=LINE('',#2653,#682);
#514=LINE('',#2654,#683);
#515=LINE('',#2657,#684);
#516=LINE('',#2659,#685);
#517=LINE('',#2660,#686);
#518=LINE('',#2662,#687);
#519=LINE('',#2663,#688);
#520=LINE('',#2665,#689);
#521=LINE('',#2666,#690);
#522=LINE('',#2673,#691);
#523=LINE('',#2675,#692);
#524=LINE('',#2677,#693);
#525=LINE('',#2678,#694);
#526=LINE('',#2681,#695);
#527=LINE('',#2683,#696);
#528=LINE('',#2684,#697);
#529=LINE('',#2687,#698);
#530=LINE('',#2689,#699);
#531=LINE('',#2690,#700);
#532=LINE('',#2693,#701);
#533=LINE('',#2695,#702);
#534=LINE('',#2696,#703);
#535=LINE('',#2699,#704);
#536=LINE('',#2701,#705);
#537=LINE('',#2702,#706);
#538=LINE('',#2705,#707);
#539=LINE('',#2707,#708);
#540=LINE('',#2708,#709);
#541=LINE('',#2711,#710);
#542=LINE('',#2713,#711);
#543=LINE('',#2714,#712);
#544=LINE('',#2716,#713);
#545=LINE('',#2717,#714);
#546=LINE('',#2724,#715);
#547=LINE('',#2726,#716);
#548=LINE('',#2728,#717);
#549=LINE('',#2729,#718);
#550=LINE('',#2732,#719);
#551=LINE('',#2734,#720);
#552=LINE('',#2735,#721);
#553=LINE('',#2738,#722);
#554=LINE('',#2740,#723);
#555=LINE('',#2741,#724);
#556=LINE('',#2743,#725);
#557=LINE('',#2744,#726);
#558=LINE('',#2752,#727);
#559=LINE('',#2757,#728);
#560=LINE('',#2762,#729);
#561=VECTOR('',#1863,6.99999999999993);
#562=VECTOR('',#1870,7.00000000000001);
#563=VECTOR('',#1877,6.99999999999996);
#564=VECTOR('',#1884,6.9999999999999);
#565=VECTOR('',#1891,21.5);
#566=VECTOR('',#1898,21.5);
#567=VECTOR('',#1905,21.5);
#568=VECTOR('',#1912,21.5);
#569=VECTOR('',#1917,1000.);
#570=VECTOR('',#1918,1000.);
#571=VECTOR('',#1919,1000.);
#572=VECTOR('',#1920,1000.);
#573=VECTOR('',#1923,1000.);
#574=VECTOR('',#1924,1000.);
#575=VECTOR('',#1925,1000.);
#576=VECTOR('',#1926,1000.);
#577=VECTOR('',#1929,1000.);
#578=VECTOR('',#1930,1000.);
#579=VECTOR('',#1931,1000.);
#580=VECTOR('',#1932,1000.);
#581=VECTOR('',#1933,1000.);
#582=VECTOR('',#1934,1000.);
#583=VECTOR('',#1935,1000.);
#584=VECTOR('',#1936,1000.);
#585=VECTOR('',#1939,1000.);
#586=VECTOR('',#1940,1000.);
#587=VECTOR('',#1941,1000.);
#588=VECTOR('',#1942,1000.);
#589=VECTOR('',#1943,1000.);
#590=VECTOR('',#1944,1000.);
#591=VECTOR('',#1945,1000.);
#592=VECTOR('',#1946,1000.);
#593=VECTOR('',#1949,1000.);
#594=VECTOR('',#1950,1000.);
#595=VECTOR('',#1951,1000.);
#596=VECTOR('',#1952,1000.);
#597=VECTOR('',#1955,1000.);
#598=VECTOR('',#1956,1000.);
#599=VECTOR('',#1957,1000.);
#600=VECTOR('',#1958,1000.);
#601=VECTOR('',#1961,1000.);
#602=VECTOR('',#1962,1000.);
#603=VECTOR('',#1963,1000.);
#604=VECTOR('',#1964,1000.);
#605=VECTOR('',#1965,1000.);
#606=VECTOR('',#1968,1000.);
#607=VECTOR('',#1969,1000.);
#608=VECTOR('',#1970,1000.);
#609=VECTOR('',#1971,1000.);
#610=VECTOR('',#1972,1000.);
#611=VECTOR('',#1975,1000.);
#612=VECTOR('',#1978,1000.);
#613=VECTOR('',#1983,1000.);
#614=VECTOR('',#1984,1000.);
#615=VECTOR('',#1985,1000.);
#616=VECTOR('',#1990,1000.);
#617=VECTOR('',#1995,1000.);
#618=VECTOR('',#2002,1000.);
#619=VECTOR('',#2003,1000.);
#620=VECTOR('',#2004,1000.);
#621=VECTOR('',#2007,1000.);
#622=VECTOR('',#2010,1000.);
#623=VECTOR('',#2015,1000.);
#624=VECTOR('',#2016,1000.);
#625=VECTOR('',#2019,1000.);
#626=VECTOR('',#2026,1000.);
#627=VECTOR('',#2027,1000.);
#628=VECTOR('',#2028,1000.);
#629=VECTOR('',#2031,1000.);
#630=VECTOR('',#2034,1000.);
#631=VECTOR('',#2039,1000.);
#632=VECTOR('',#2040,1000.);
#633=VECTOR('',#2049,1000.);
#634=VECTOR('',#2052,1000.);
#635=VECTOR('',#2057,1000.);
#636=VECTOR('',#2058,1000.);
#637=VECTOR('',#2061,1000.);
#638=VECTOR('',#2064,1000.);
#639=VECTOR('',#2067,1000.);
#640=VECTOR('',#2070,1000.);
#641=VECTOR('',#2073,1000.);
#642=VECTOR('',#2076,1000.);
#643=VECTOR('',#2081,1000.);
#644=VECTOR('',#2084,1000.);
#645=VECTOR('',#2087,1000.);
#646=VECTOR('',#2090,1000.);
#647=VECTOR('',#2093,1000.);
#648=VECTOR('',#2096,1000.);
#649=VECTOR('',#2101,1000.);
#650=VECTOR('',#2102,1000.);
#651=VECTOR('',#2105,1000.);
#652=VECTOR('',#2106,1000.);
#653=VECTOR('',#2109,1000.);
#654=VECTOR('',#2110,1000.);
#655=VECTOR('',#2113,1000.);
#656=VECTOR('',#2118,1000.);
#657=VECTOR('',#2119,1000.);
#658=VECTOR('',#2122,1000.);
#659=VECTOR('',#2127,1000.);
#660=VECTOR('',#2128,1000.);
#661=VECTOR('',#2131,1000.);
#662=VECTOR('',#2136,1000.);
#663=VECTOR('',#2137,1000.);
#664=VECTOR('',#2140,1000.);
#665=VECTOR('',#2149,21.5000000000002);
#666=VECTOR('',#2156,21.5000000000002);
#667=VECTOR('',#2161,1000.);
#668=VECTOR('',#2162,1000.);
#669=VECTOR('',#2163,1000.);
#670=VECTOR('',#2164,1000.);
#671=VECTOR('',#2167,1000.);
#672=VECTOR('',#2168,1000.);
#673=VECTOR('',#2169,1000.);
#674=VECTOR('',#2172,1000.);
#675=VECTOR('',#2173,1000.);
#676=VECTOR('',#2174,1000.);
#677=VECTOR('',#2177,1000.);
#678=VECTOR('',#2178,1000.);
#679=VECTOR('',#2179,1000.);
#680=VECTOR('',#2180,1000.);
#681=VECTOR('',#2183,1000.);
#682=VECTOR('',#2184,1000.);
#683=VECTOR('',#2185,1000.);
#684=VECTOR('',#2188,1000.);
#685=VECTOR('',#2189,1000.);
#686=VECTOR('',#2190,1000.);
#687=VECTOR('',#2193,1000.);
#688=VECTOR('',#2194,1000.);
#689=VECTOR('',#2197,1000.);
#690=VECTOR('',#2198,1000.);
#691=VECTOR('',#2207,1000.);
#692=VECTOR('',#2208,1000.);
#693=VECTOR('',#2209,1000.);
#694=VECTOR('',#2210,1000.);
#695=VECTOR('',#2213,1000.);
#696=VECTOR('',#2214,1000.);
#697=VECTOR('',#2215,1000.);
#698=VECTOR('',#2218,1000.);
#699=VECTOR('',#2219,1000.);
#700=VECTOR('',#2220,1000.);
#701=VECTOR('',#2223,1000.);
#702=VECTOR('',#2224,1000.);
#703=VECTOR('',#2225,1000.);
#704=VECTOR('',#2228,1000.);
#705=VECTOR('',#2229,1000.);
#706=VECTOR('',#2230,1000.);
#707=VECTOR('',#2233,1000.);
#708=VECTOR('',#2234,1000.);
#709=VECTOR('',#2235,1000.);
#710=VECTOR('',#2238,1000.);
#711=VECTOR('',#2239,1000.);
#712=VECTOR('',#2240,1000.);
#713=VECTOR('',#2243,1000.);
#714=VECTOR('',#2244,1000.);
#715=VECTOR('',#2253,1000.);
#716=VECTOR('',#2254,1000.);
#717=VECTOR('',#2255,1000.);
#718=VECTOR('',#2256,1000.);
#719=VECTOR('',#2259,1000.);
#720=VECTOR('',#2260,1000.);
#721=VECTOR('',#2261,1000.);
#722=VECTOR('',#2264,1000.);
#723=VECTOR('',#2265,1000.);
#724=VECTOR('',#2266,1000.);
#725=VECTOR('',#2269,1000.);
#726=VECTOR('',#2270,1000.);
#727=VECTOR('',#2281,18.6799999999998);
#728=VECTOR('',#2288,17.6799999999998);
#729=VECTOR('',#2293,21.0799999999997);
#730=CIRCLE('',#1705,6.99999999999992);
#731=CIRCLE('',#1706,6.99999999999992);
#732=CIRCLE('',#1708,7.00000000000001);
#733=CIRCLE('',#1709,7.00000000000001);
#734=CIRCLE('',#1711,6.99999999999996);
#735=CIRCLE('',#1712,6.99999999999996);
#736=CIRCLE('',#1714,6.9999999999999);
#737=CIRCLE('',#1715,6.9999999999999);
#738=CIRCLE('',#1717,21.5);
#739=CIRCLE('',#1718,21.5);
#740=CIRCLE('',#1720,21.5);
#741=CIRCLE('',#1721,21.5);
#742=CIRCLE('',#1723,21.5);
#743=CIRCLE('',#1724,21.5);
#744=CIRCLE('',#1726,21.5);
#745=CIRCLE('',#1727,21.5);
#746=CIRCLE('',#1737,7.35);
#747=CIRCLE('',#1738,1.);
#748=CIRCLE('',#1741,7.35);
#749=CIRCLE('',#1742,1.);
#750=CIRCLE('',#1744,1.);
#751=CIRCLE('',#1745,7.35000000000002);
#752=CIRCLE('',#1748,1.);
#753=CIRCLE('',#1749,7.35000000000002);
#754=CIRCLE('',#1752,1.);
#755=CIRCLE('',#1753,7.35000000000002);
#756=CIRCLE('',#1756,1.);
#757=CIRCLE('',#1757,7.35000000000002);
#758=CIRCLE('',#1760,7.34999999999997);
#759=CIRCLE('',#1761,1.);
#760=CIRCLE('',#1763,7.34999999999997);
#761=CIRCLE('',#1764,1.);
#762=CIRCLE('',#1796,21.5000000000002);
#763=CIRCLE('',#1797,21.5000000000002);
#764=CIRCLE('',#1799,21.5000000000002);
#765=CIRCLE('',#1800,21.5000000000002);
#766=CIRCLE('',#1831,17.6799999999998);
#767=CIRCLE('',#1832,18.6799999999998);
#768=CIRCLE('',#1834,17.6799999999998);
#769=CIRCLE('',#1836,21.0799999999997);
#770=CIRCLE('',#1837,21.0799999999997);
#771=VERTEX_POINT('',#2333);
#772=VERTEX_POINT('',#2335);
#773=VERTEX_POINT('',#2339);
#774=VERTEX_POINT('',#2341);
#775=VERTEX_POINT('',#2345);
#776=VERTEX_POINT('',#2347);
#777=VERTEX_POINT('',#2351);
#778=VERTEX_POINT('',#2353);
#779=VERTEX_POINT('',#2357);
#780=VERTEX_POINT('',#2359);
#781=VERTEX_POINT('',#2363);
#782=VERTEX_POINT('',#2365);
#783=VERTEX_POINT('',#2369);
#784=VERTEX_POINT('',#2371);
#785=VERTEX_POINT('',#2375);
#786=VERTEX_POINT('',#2377);
#787=VERTEX_POINT('',#2381);
#788=VERTEX_POINT('',#2382);
#789=VERTEX_POINT('',#2384);
#790=VERTEX_POINT('',#2386);
#791=VERTEX_POINT('',#2390);
#792=VERTEX_POINT('',#2391);
#793=VERTEX_POINT('',#2393);
#794=VERTEX_POINT('',#2395);
#795=VERTEX_POINT('',#2399);
#796=VERTEX_POINT('',#2400);
#797=VERTEX_POINT('',#2402);
#798=VERTEX_POINT('',#2404);
#799=VERTEX_POINT('',#2406);
#800=VERTEX_POINT('',#2408);
#801=VERTEX_POINT('',#2410);
#802=VERTEX_POINT('',#2412);
#803=VERTEX_POINT('',#2416);
#804=VERTEX_POINT('',#2417);
#805=VERTEX_POINT('',#2419);
#806=VERTEX_POINT('',#2421);
#807=VERTEX_POINT('',#2423);
#808=VERTEX_POINT('',#2425);
#809=VERTEX_POINT('',#2427);
#810=VERTEX_POINT('',#2429);
#811=VERTEX_POINT('',#2433);
#812=VERTEX_POINT('',#2434);
#813=VERTEX_POINT('',#2440);
#814=VERTEX_POINT('',#2441);
#815=VERTEX_POINT('',#2447);
#816=VERTEX_POINT('',#2450);
#817=VERTEX_POINT('',#2452);
#818=VERTEX_POINT('',#2456);
#819=VERTEX_POINT('',#2457);
#820=VERTEX_POINT('',#2460);
#821=VERTEX_POINT('',#2465);
#822=VERTEX_POINT('',#2466);
#823=VERTEX_POINT('',#2472);
#824=VERTEX_POINT('',#2474);
#825=VERTEX_POINT('',#2478);
#826=VERTEX_POINT('',#2480);
#827=VERTEX_POINT('',#2484);
#828=VERTEX_POINT('',#2485);
#829=VERTEX_POINT('',#2490);
#830=VERTEX_POINT('',#2492);
#831=VERTEX_POINT('',#2496);
#832=VERTEX_POINT('',#2497);
#833=VERTEX_POINT('',#2499);
#834=VERTEX_POINT('',#2501);
#835=VERTEX_POINT('',#2508);
#836=VERTEX_POINT('',#2509);
#837=VERTEX_POINT('',#2514);
#838=VERTEX_POINT('',#2516);
#839=VERTEX_POINT('',#2520);
#840=VERTEX_POINT('',#2521);
#841=VERTEX_POINT('',#2523);
#842=VERTEX_POINT('',#2525);
#843=VERTEX_POINT('',#2535);
#844=VERTEX_POINT('',#2536);
#845=VERTEX_POINT('',#2571);
#846=VERTEX_POINT('',#2575);
#847=VERTEX_POINT('',#2579);
#848=VERTEX_POINT('',#2586);
#849=VERTEX_POINT('',#2593);
#850=VERTEX_POINT('',#2600);
#851=VERTEX_POINT('',#2608);
#852=VERTEX_POINT('',#2610);
#853=VERTEX_POINT('',#2614);
#854=VERTEX_POINT('',#2616);
#855=VERTEX_POINT('',#2620);
#856=VERTEX_POINT('',#2621);
#857=VERTEX_POINT('',#2623);
#858=VERTEX_POINT('',#2625);
#859=VERTEX_POINT('',#2629);
#860=VERTEX_POINT('',#2631);
#861=VERTEX_POINT('',#2635);
#862=VERTEX_POINT('',#2637);
#863=VERTEX_POINT('',#2641);
#864=VERTEX_POINT('',#2642);
#865=VERTEX_POINT('',#2644);
#866=VERTEX_POINT('',#2646);
#867=VERTEX_POINT('',#2650);
#868=VERTEX_POINT('',#2652);
#869=VERTEX_POINT('',#2656);
#870=VERTEX_POINT('',#2658);
#871=VERTEX_POINT('',#2671);
#872=VERTEX_POINT('',#2672);
#873=VERTEX_POINT('',#2674);
#874=VERTEX_POINT('',#2676);
#875=VERTEX_POINT('',#2680);
#876=VERTEX_POINT('',#2682);
#877=VERTEX_POINT('',#2686);
#878=VERTEX_POINT('',#2688);
#879=VERTEX_POINT('',#2692);
#880=VERTEX_POINT('',#2694);
#881=VERTEX_POINT('',#2698);
#882=VERTEX_POINT('',#2700);
#883=VERTEX_POINT('',#2704);
#884=VERTEX_POINT('',#2706);
#885=VERTEX_POINT('',#2710);
#886=VERTEX_POINT('',#2712);
#887=VERTEX_POINT('',#2722);
#888=VERTEX_POINT('',#2723);
#889=VERTEX_POINT('',#2725);
#890=VERTEX_POINT('',#2727);
#891=VERTEX_POINT('',#2731);
#892=VERTEX_POINT('',#2733);
#893=VERTEX_POINT('',#2737);
#894=VERTEX_POINT('',#2739);
#895=VERTEX_POINT('',#2749);
#896=VERTEX_POINT('',#2751);
#897=VERTEX_POINT('',#2755);
#898=VERTEX_POINT('',#2759);
#899=VERTEX_POINT('',#2761);
#900=EDGE_CURVE('',#771,#771,#730,.T.);
#901=EDGE_CURVE('',#771,#772,#392,.T.);
#902=EDGE_CURVE('',#772,#772,#731,.T.);
#903=EDGE_CURVE('',#773,#773,#732,.T.);
#904=EDGE_CURVE('',#773,#774,#393,.T.);
#905=EDGE_CURVE('',#774,#774,#733,.T.);
#906=EDGE_CURVE('',#775,#775,#734,.T.);
#907=EDGE_CURVE('',#775,#776,#394,.T.);
#908=EDGE_CURVE('',#776,#776,#735,.T.);
#909=EDGE_CURVE('',#777,#777,#736,.T.);
#910=EDGE_CURVE('',#777,#778,#395,.T.);
#911=EDGE_CURVE('',#778,#778,#737,.T.);
#912=EDGE_CURVE('',#779,#779,#738,.T.);
#913=EDGE_CURVE('',#779,#780,#396,.T.);
#914=EDGE_CURVE('',#780,#780,#739,.T.);
#915=EDGE_CURVE('',#781,#781,#740,.T.);
#916=EDGE_CURVE('',#781,#782,#397,.T.);
#917=EDGE_CURVE('',#782,#782,#741,.T.);
#918=EDGE_CURVE('',#783,#783,#742,.T.);
#919=EDGE_CURVE('',#783,#784,#398,.T.);
#920=EDGE_CURVE('',#784,#784,#743,.T.);
#921=EDGE_CURVE('',#785,#785,#744,.T.);
#922=EDGE_CURVE('',#785,#786,#399,.T.);
#923=EDGE_CURVE('',#786,#786,#745,.T.);
#924=EDGE_CURVE('',#787,#788,#400,.T.);
#925=EDGE_CURVE('',#789,#788,#401,.T.);
#926=EDGE_CURVE('',#790,#789,#402,.T.);
#927=EDGE_CURVE('',#790,#787,#403,.T.);
#928=EDGE_CURVE('',#791,#792,#404,.T.);
#929=EDGE_CURVE('',#793,#792,#405,.T.);
#930=EDGE_CURVE('',#794,#793,#406,.T.);
#931=EDGE_CURVE('',#794,#791,#407,.T.);
#932=EDGE_CURVE('',#795,#796,#408,.T.);
#933=EDGE_CURVE('',#796,#797,#409,.T.);
#934=EDGE_CURVE('',#798,#797,#410,.T.);
#935=EDGE_CURVE('',#798,#799,#411,.T.);
#936=EDGE_CURVE('',#799,#800,#412,.T.);
#937=EDGE_CURVE('',#801,#800,#413,.T.);
#938=EDGE_CURVE('',#802,#801,#414,.T.);
#939=EDGE_CURVE('',#795,#802,#415,.T.);
#940=EDGE_CURVE('',#803,#804,#416,.T.);
#941=EDGE_CURVE('',#803,#805,#417,.T.);
#942=EDGE_CURVE('',#806,#805,#418,.T.);
#943=EDGE_CURVE('',#806,#807,#419,.T.);
#944=EDGE_CURVE('',#807,#808,#420,.T.);
#945=EDGE_CURVE('',#809,#808,#421,.T.);
#946=EDGE_CURVE('',#809,#810,#422,.T.);
#947=EDGE_CURVE('',#804,#810,#423,.T.);
#948=EDGE_CURVE('',#811,#812,#424,.T.);
#949=EDGE_CURVE('',#811,#809,#425,.T.);
#950=EDGE_CURVE('',#808,#792,#426,.T.);
#951=EDGE_CURVE('',#791,#812,#427,.T.);
#952=EDGE_CURVE('',#813,#814,#428,.T.);
#953=EDGE_CURVE('',#814,#796,#429,.T.);
#954=EDGE_CURVE('',#795,#790,#430,.T.);
#955=EDGE_CURVE('',#813,#789,#431,.T.);
#956=EDGE_CURVE('',#815,#798,#432,.T.);
#957=EDGE_CURVE('',#813,#815,#433,.T.);
#958=EDGE_CURVE('',#816,#788,#434,.T.);
#959=EDGE_CURVE('',#816,#817,#435,.T.);
#960=EDGE_CURVE('',#817,#799,#436,.T.);
#961=EDGE_CURVE('',#818,#819,#437,.T.);
#962=EDGE_CURVE('',#818,#803,#438,.T.);
#963=EDGE_CURVE('',#820,#804,#439,.T.);
#964=EDGE_CURVE('',#812,#820,#440,.T.);
#965=EDGE_CURVE('',#794,#819,#441,.T.);
#966=EDGE_CURVE('',#821,#822,#442,.T.);
#967=EDGE_CURVE('',#807,#821,#746,.T.);
#968=EDGE_CURVE('',#793,#807,#443,.T.);
#969=EDGE_CURVE('',#793,#822,#747,.T.);
#970=EDGE_CURVE('',#821,#823,#444,.T.);
#971=EDGE_CURVE('',#822,#824,#445,.T.);
#972=EDGE_CURVE('',#824,#823,#446,.T.);
#973=EDGE_CURVE('',#808,#825,#748,.T.);
#974=EDGE_CURVE('',#826,#825,#447,.T.);
#975=EDGE_CURVE('',#792,#826,#749,.T.);
#976=EDGE_CURVE('',#827,#828,#448,.T.);
#977=EDGE_CURVE('',#823,#827,#750,.T.);
#978=EDGE_CURVE('',#824,#828,#751,.T.);
#979=EDGE_CURVE('',#827,#829,#449,.T.);
#980=EDGE_CURVE('',#828,#830,#450,.T.);
#981=EDGE_CURVE('',#830,#829,#451,.T.);
#982=EDGE_CURVE('',#831,#832,#452,.T.);
#983=EDGE_CURVE('',#831,#833,#752,.T.);
#984=EDGE_CURVE('',#834,#833,#453,.T.);
#985=EDGE_CURVE('',#832,#834,#753,.T.);
#986=EDGE_CURVE('',#825,#831,#454,.T.);
#987=EDGE_CURVE('',#826,#832,#455,.T.);
#988=EDGE_CURVE('',#835,#836,#456,.T.);
#989=EDGE_CURVE('',#829,#835,#754,.T.);
#990=EDGE_CURVE('',#830,#836,#755,.T.);
#991=EDGE_CURVE('',#835,#837,#457,.T.);
#992=EDGE_CURVE('',#836,#838,#458,.T.);
#993=EDGE_CURVE('',#838,#837,#459,.T.);
#994=EDGE_CURVE('',#839,#840,#460,.T.);
#995=EDGE_CURVE('',#839,#841,#756,.T.);
#996=EDGE_CURVE('',#842,#841,#461,.T.);
#997=EDGE_CURVE('',#840,#842,#757,.T.);
#998=EDGE_CURVE('',#833,#839,#462,.T.);
#999=EDGE_CURVE('',#834,#840,#463,.T.);
#1000=EDGE_CURVE('',#837,#795,#758,.T.);
#1001=EDGE_CURVE('',#838,#790,#759,.T.);
#1002=EDGE_CURVE('',#843,#844,#464,.T.);
#1003=EDGE_CURVE('',#843,#802,#760,.T.);
#1004=EDGE_CURVE('',#787,#802,#465,.T.);
#1005=EDGE_CURVE('',#844,#787,#761,.T.);
#1006=EDGE_CURVE('',#841,#843,#466,.T.);
#1007=EDGE_CURVE('',#842,#844,#467,.T.);
#1008=EDGE_CURVE('',#837,#843,#468,.T.);
#1009=EDGE_CURVE('',#835,#841,#469,.T.);
#1010=EDGE_CURVE('',#829,#839,#470,.T.);
#1011=EDGE_CURVE('',#827,#833,#471,.T.);
#1012=EDGE_CURVE('',#823,#831,#472,.T.);
#1013=EDGE_CURVE('',#821,#825,#473,.T.);
#1014=EDGE_CURVE('',#822,#826,#474,.T.);
#1015=EDGE_CURVE('',#824,#832,#475,.T.);
#1016=EDGE_CURVE('',#828,#834,#476,.T.);
#1017=EDGE_CURVE('',#830,#840,#477,.T.);
#1018=EDGE_CURVE('',#836,#842,#478,.T.);
#1019=EDGE_CURVE('',#838,#844,#479,.T.);
#1020=EDGE_CURVE('',#845,#806,#480,.T.);
#1021=EDGE_CURVE('',#819,#845,#481,.T.);
#1022=EDGE_CURVE('',#846,#801,#482,.T.);
#1023=EDGE_CURVE('',#816,#846,#483,.T.);
#1024=EDGE_CURVE('',#817,#847,#484,.T.);
#1025=EDGE_CURVE('',#847,#800,#485,.T.);
#1026=EDGE_CURVE('',#846,#847,#486,.T.);
#1027=EDGE_CURVE('',#818,#848,#487,.T.);
#1028=EDGE_CURVE('',#848,#805,#488,.T.);
#1029=EDGE_CURVE('',#845,#848,#489,.T.);
#1030=EDGE_CURVE('',#811,#849,#490,.T.);
#1031=EDGE_CURVE('',#849,#810,#491,.T.);
#1032=EDGE_CURVE('',#820,#849,#492,.T.);
#1033=EDGE_CURVE('',#814,#850,#493,.T.);
#1034=EDGE_CURVE('',#850,#797,#494,.T.);
#1035=EDGE_CURVE('',#815,#850,#495,.T.);
#1036=EDGE_CURVE('',#851,#851,#762,.T.);
#1037=EDGE_CURVE('',#851,#852,#496,.T.);
#1038=EDGE_CURVE('',#852,#852,#763,.T.);
#1039=EDGE_CURVE('',#853,#853,#764,.T.);
#1040=EDGE_CURVE('',#853,#854,#497,.T.);
#1041=EDGE_CURVE('',#854,#854,#765,.T.);
#1042=EDGE_CURVE('',#855,#856,#498,.T.);
#1043=EDGE_CURVE('',#857,#856,#499,.T.);
#1044=EDGE_CURVE('',#858,#857,#500,.T.);
#1045=EDGE_CURVE('',#858,#855,#501,.T.);
#1046=EDGE_CURVE('',#856,#859,#502,.T.);
#1047=EDGE_CURVE('',#860,#859,#503,.T.);
#1048=EDGE_CURVE('',#857,#860,#504,.T.);
#1049=EDGE_CURVE('',#859,#861,#505,.T.);
#1050=EDGE_CURVE('',#862,#861,#506,.T.);
#1051=EDGE_CURVE('',#860,#862,#507,.T.);
#1052=EDGE_CURVE('',#863,#864,#508,.T.);
#1053=EDGE_CURVE('',#865,#863,#509,.T.);
#1054=EDGE_CURVE('',#865,#866,#510,.T.);
#1055=EDGE_CURVE('',#866,#864,#511,.T.);
#1056=EDGE_CURVE('',#867,#863,#512,.T.);
#1057=EDGE_CURVE('',#868,#867,#513,.T.);
#1058=EDGE_CURVE('',#868,#865,#514,.T.);
#1059=EDGE_CURVE('',#869,#867,#515,.T.);
#1060=EDGE_CURVE('',#870,#869,#516,.T.);
#1061=EDGE_CURVE('',#870,#868,#517,.T.);
#1062=EDGE_CURVE('',#864,#869,#518,.T.);
#1063=EDGE_CURVE('',#866,#870,#519,.T.);
#1064=EDGE_CURVE('',#861,#855,#520,.T.);
#1065=EDGE_CURVE('',#862,#858,#521,.T.);
#1066=EDGE_CURVE('',#871,#872,#522,.T.);
#1067=EDGE_CURVE('',#873,#872,#523,.T.);
#1068=EDGE_CURVE('',#874,#873,#524,.T.);
#1069=EDGE_CURVE('',#874,#871,#525,.T.);
#1070=EDGE_CURVE('',#872,#875,#526,.T.);
#1071=EDGE_CURVE('',#876,#875,#527,.T.);
#1072=EDGE_CURVE('',#873,#876,#528,.T.);
#1073=EDGE_CURVE('',#875,#877,#529,.T.);
#1074=EDGE_CURVE('',#878,#877,#530,.T.);
#1075=EDGE_CURVE('',#876,#878,#531,.T.);
#1076=EDGE_CURVE('',#877,#879,#532,.T.);
#1077=EDGE_CURVE('',#880,#879,#533,.T.);
#1078=EDGE_CURVE('',#878,#880,#534,.T.);
#1079=EDGE_CURVE('',#879,#881,#535,.T.);
#1080=EDGE_CURVE('',#882,#881,#536,.T.);
#1081=EDGE_CURVE('',#880,#882,#537,.T.);
#1082=EDGE_CURVE('',#881,#883,#538,.T.);
#1083=EDGE_CURVE('',#884,#883,#539,.T.);
#1084=EDGE_CURVE('',#882,#884,#540,.T.);
#1085=EDGE_CURVE('',#883,#885,#541,.T.);
#1086=EDGE_CURVE('',#886,#885,#542,.T.);
#1087=EDGE_CURVE('',#884,#886,#543,.T.);
#1088=EDGE_CURVE('',#885,#871,#544,.T.);
#1089=EDGE_CURVE('',#886,#874,#545,.T.);
#1090=EDGE_CURVE('',#887,#888,#546,.T.);
#1091=EDGE_CURVE('',#889,#888,#547,.T.);
#1092=EDGE_CURVE('',#890,#889,#548,.T.);
#1093=EDGE_CURVE('',#890,#887,#549,.T.);
#1094=EDGE_CURVE('',#888,#891,#550,.T.);
#1095=EDGE_CURVE('',#892,#891,#551,.T.);
#1096=EDGE_CURVE('',#889,#892,#552,.T.);
#1097=EDGE_CURVE('',#891,#893,#553,.T.);
#1098=EDGE_CURVE('',#894,#893,#554,.T.);
#1099=EDGE_CURVE('',#892,#894,#555,.T.);
#1100=EDGE_CURVE('',#893,#887,#556,.T.);
#1101=EDGE_CURVE('',#894,#890,#557,.T.);
#1102=EDGE_CURVE('',#895,#895,#766,.T.);
#1103=EDGE_CURVE('',#895,#896,#558,.T.);
#1104=EDGE_CURVE('',#896,#896,#767,.T.);
#1105=EDGE_CURVE('',#897,#897,#768,.T.);
#1106=EDGE_CURVE('',#897,#895,#559,.T.);
#1107=EDGE_CURVE('',#898,#898,#769,.T.);
#1108=EDGE_CURVE('',#898,#899,#560,.T.);
#1109=EDGE_CURVE('',#899,#899,#770,.T.);
#1110=ORIENTED_EDGE('',*,*,#900,.F.);
#1111=ORIENTED_EDGE('',*,*,#901,.T.);
#1112=ORIENTED_EDGE('',*,*,#902,.T.);
#1113=ORIENTED_EDGE('',*,*,#901,.F.);
#1114=ORIENTED_EDGE('',*,*,#903,.F.);
#1115=ORIENTED_EDGE('',*,*,#904,.T.);
#1116=ORIENTED_EDGE('',*,*,#905,.T.);
#1117=ORIENTED_EDGE('',*,*,#904,.F.);
#1118=ORIENTED_EDGE('',*,*,#906,.T.);
#1119=ORIENTED_EDGE('',*,*,#907,.T.);
#1120=ORIENTED_EDGE('',*,*,#908,.F.);
#1121=ORIENTED_EDGE('',*,*,#907,.F.);
#1122=ORIENTED_EDGE('',*,*,#909,.T.);
#1123=ORIENTED_EDGE('',*,*,#910,.T.);
#1124=ORIENTED_EDGE('',*,*,#911,.F.);
#1125=ORIENTED_EDGE('',*,*,#910,.F.);
#1126=ORIENTED_EDGE('',*,*,#912,.T.);
#1127=ORIENTED_EDGE('',*,*,#913,.T.);
#1128=ORIENTED_EDGE('',*,*,#914,.F.);
#1129=ORIENTED_EDGE('',*,*,#913,.F.);
#1130=ORIENTED_EDGE('',*,*,#915,.F.);
#1131=ORIENTED_EDGE('',*,*,#916,.T.);
#1132=ORIENTED_EDGE('',*,*,#917,.T.);
#1133=ORIENTED_EDGE('',*,*,#916,.F.);
#1134=ORIENTED_EDGE('',*,*,#918,.T.);
#1135=ORIENTED_EDGE('',*,*,#919,.T.);
#1136=ORIENTED_EDGE('',*,*,#920,.F.);
#1137=ORIENTED_EDGE('',*,*,#919,.F.);
#1138=ORIENTED_EDGE('',*,*,#921,.F.);
#1139=ORIENTED_EDGE('',*,*,#922,.T.);
#1140=ORIENTED_EDGE('',*,*,#923,.T.);
#1141=ORIENTED_EDGE('',*,*,#922,.F.);
#1142=ORIENTED_EDGE('',*,*,#924,.T.);
#1143=ORIENTED_EDGE('',*,*,#925,.F.);
#1144=ORIENTED_EDGE('',*,*,#926,.F.);
#1145=ORIENTED_EDGE('',*,*,#927,.T.);
#1146=ORIENTED_EDGE('',*,*,#915,.T.);
#1147=ORIENTED_EDGE('',*,*,#902,.F.);
#1148=ORIENTED_EDGE('',*,*,#911,.T.);
#1149=ORIENTED_EDGE('',*,*,#912,.F.);
#1150=ORIENTED_EDGE('',*,*,#928,.T.);
#1151=ORIENTED_EDGE('',*,*,#929,.F.);
#1152=ORIENTED_EDGE('',*,*,#930,.F.);
#1153=ORIENTED_EDGE('',*,*,#931,.T.);
#1154=ORIENTED_EDGE('',*,*,#921,.T.);
#1155=ORIENTED_EDGE('',*,*,#905,.F.);
#1156=ORIENTED_EDGE('',*,*,#908,.T.);
#1157=ORIENTED_EDGE('',*,*,#918,.F.);
#1158=ORIENTED_EDGE('',*,*,#932,.T.);
#1159=ORIENTED_EDGE('',*,*,#933,.T.);
#1160=ORIENTED_EDGE('',*,*,#934,.F.);
#1161=ORIENTED_EDGE('',*,*,#935,.T.);
#1162=ORIENTED_EDGE('',*,*,#936,.T.);
#1163=ORIENTED_EDGE('',*,*,#937,.F.);
#1164=ORIENTED_EDGE('',*,*,#938,.F.);
#1165=ORIENTED_EDGE('',*,*,#939,.F.);
#1166=ORIENTED_EDGE('',*,*,#917,.F.);
#1167=ORIENTED_EDGE('',*,*,#914,.T.);
#1168=ORIENTED_EDGE('',*,*,#940,.F.);
#1169=ORIENTED_EDGE('',*,*,#941,.T.);
#1170=ORIENTED_EDGE('',*,*,#942,.F.);
#1171=ORIENTED_EDGE('',*,*,#943,.T.);
#1172=ORIENTED_EDGE('',*,*,#944,.T.);
#1173=ORIENTED_EDGE('',*,*,#945,.F.);
#1174=ORIENTED_EDGE('',*,*,#946,.T.);
#1175=ORIENTED_EDGE('',*,*,#947,.F.);
#1176=ORIENTED_EDGE('',*,*,#923,.F.);
#1177=ORIENTED_EDGE('',*,*,#920,.T.);
#1178=ORIENTED_EDGE('',*,*,#948,.F.);
#1179=ORIENTED_EDGE('',*,*,#949,.T.);
#1180=ORIENTED_EDGE('',*,*,#945,.T.);
#1181=ORIENTED_EDGE('',*,*,#950,.T.);
#1182=ORIENTED_EDGE('',*,*,#928,.F.);
#1183=ORIENTED_EDGE('',*,*,#951,.T.);
#1184=ORIENTED_EDGE('',*,*,#952,.T.);
#1185=ORIENTED_EDGE('',*,*,#953,.T.);
#1186=ORIENTED_EDGE('',*,*,#932,.F.);
#1187=ORIENTED_EDGE('',*,*,#954,.T.);
#1188=ORIENTED_EDGE('',*,*,#926,.T.);
#1189=ORIENTED_EDGE('',*,*,#955,.F.);
#1190=ORIENTED_EDGE('',*,*,#956,.F.);
#1191=ORIENTED_EDGE('',*,*,#957,.F.);
#1192=ORIENTED_EDGE('',*,*,#955,.T.);
#1193=ORIENTED_EDGE('',*,*,#925,.T.);
#1194=ORIENTED_EDGE('',*,*,#958,.F.);
#1195=ORIENTED_EDGE('',*,*,#959,.T.);
#1196=ORIENTED_EDGE('',*,*,#960,.T.);
#1197=ORIENTED_EDGE('',*,*,#935,.F.);
#1198=ORIENTED_EDGE('',*,*,#961,.F.);
#1199=ORIENTED_EDGE('',*,*,#962,.T.);
#1200=ORIENTED_EDGE('',*,*,#940,.T.);
#1201=ORIENTED_EDGE('',*,*,#963,.F.);
#1202=ORIENTED_EDGE('',*,*,#964,.F.);
#1203=ORIENTED_EDGE('',*,*,#951,.F.);
#1204=ORIENTED_EDGE('',*,*,#931,.F.);
#1205=ORIENTED_EDGE('',*,*,#965,.T.);
#1206=ORIENTED_EDGE('',*,*,#966,.F.);
#1207=ORIENTED_EDGE('',*,*,#967,.F.);
#1208=ORIENTED_EDGE('',*,*,#968,.F.);
#1209=ORIENTED_EDGE('',*,*,#969,.T.);
#1210=ORIENTED_EDGE('',*,*,#970,.F.);
#1211=ORIENTED_EDGE('',*,*,#966,.T.);
#1212=ORIENTED_EDGE('',*,*,#971,.T.);
#1213=ORIENTED_EDGE('',*,*,#972,.T.);
#1214=ORIENTED_EDGE('',*,*,#950,.F.);
#1215=ORIENTED_EDGE('',*,*,#973,.T.);
#1216=ORIENTED_EDGE('',*,*,#974,.F.);
#1217=ORIENTED_EDGE('',*,*,#975,.F.);
#1218=ORIENTED_EDGE('',*,*,#976,.F.);
#1219=ORIENTED_EDGE('',*,*,#977,.F.);
#1220=ORIENTED_EDGE('',*,*,#972,.F.);
#1221=ORIENTED_EDGE('',*,*,#978,.T.);
#1222=ORIENTED_EDGE('',*,*,#979,.F.);
#1223=ORIENTED_EDGE('',*,*,#976,.T.);
#1224=ORIENTED_EDGE('',*,*,#980,.T.);
#1225=ORIENTED_EDGE('',*,*,#981,.T.);
#1226=ORIENTED_EDGE('',*,*,#982,.F.);
#1227=ORIENTED_EDGE('',*,*,#983,.T.);
#1228=ORIENTED_EDGE('',*,*,#984,.F.);
#1229=ORIENTED_EDGE('',*,*,#985,.F.);
#1230=ORIENTED_EDGE('',*,*,#986,.T.);
#1231=ORIENTED_EDGE('',*,*,#982,.T.);
#1232=ORIENTED_EDGE('',*,*,#987,.F.);
#1233=ORIENTED_EDGE('',*,*,#974,.T.);
#1234=ORIENTED_EDGE('',*,*,#988,.F.);
#1235=ORIENTED_EDGE('',*,*,#989,.F.);
#1236=ORIENTED_EDGE('',*,*,#981,.F.);
#1237=ORIENTED_EDGE('',*,*,#990,.T.);
#1238=ORIENTED_EDGE('',*,*,#991,.F.);
#1239=ORIENTED_EDGE('',*,*,#988,.T.);
#1240=ORIENTED_EDGE('',*,*,#992,.T.);
#1241=ORIENTED_EDGE('',*,*,#993,.T.);
#1242=ORIENTED_EDGE('',*,*,#994,.F.);
#1243=ORIENTED_EDGE('',*,*,#995,.T.);
#1244=ORIENTED_EDGE('',*,*,#996,.F.);
#1245=ORIENTED_EDGE('',*,*,#997,.F.);
#1246=ORIENTED_EDGE('',*,*,#998,.T.);
#1247=ORIENTED_EDGE('',*,*,#994,.T.);
#1248=ORIENTED_EDGE('',*,*,#999,.F.);
#1249=ORIENTED_EDGE('',*,*,#984,.T.);
#1250=ORIENTED_EDGE('',*,*,#954,.F.);
#1251=ORIENTED_EDGE('',*,*,#1000,.F.);
#1252=ORIENTED_EDGE('',*,*,#993,.F.);
#1253=ORIENTED_EDGE('',*,*,#1001,.T.);
#1254=ORIENTED_EDGE('',*,*,#1002,.F.);
#1255=ORIENTED_EDGE('',*,*,#1003,.T.);
#1256=ORIENTED_EDGE('',*,*,#1004,.F.);
#1257=ORIENTED_EDGE('',*,*,#1005,.F.);
#1258=ORIENTED_EDGE('',*,*,#1006,.T.);
#1259=ORIENTED_EDGE('',*,*,#1002,.T.);
#1260=ORIENTED_EDGE('',*,*,#1007,.F.);
#1261=ORIENTED_EDGE('',*,*,#996,.T.);
#1262=ORIENTED_EDGE('',*,*,#1003,.F.);
#1263=ORIENTED_EDGE('',*,*,#1008,.F.);
#1264=ORIENTED_EDGE('',*,*,#1000,.T.);
#1265=ORIENTED_EDGE('',*,*,#939,.T.);
#1266=ORIENTED_EDGE('',*,*,#1006,.F.);
#1267=ORIENTED_EDGE('',*,*,#1009,.F.);
#1268=ORIENTED_EDGE('',*,*,#991,.T.);
#1269=ORIENTED_EDGE('',*,*,#1008,.T.);
#1270=ORIENTED_EDGE('',*,*,#995,.F.);
#1271=ORIENTED_EDGE('',*,*,#1010,.F.);
#1272=ORIENTED_EDGE('',*,*,#989,.T.);
#1273=ORIENTED_EDGE('',*,*,#1009,.T.);
#1274=ORIENTED_EDGE('',*,*,#998,.F.);
#1275=ORIENTED_EDGE('',*,*,#1011,.F.);
#1276=ORIENTED_EDGE('',*,*,#979,.T.);
#1277=ORIENTED_EDGE('',*,*,#1010,.T.);
#1278=ORIENTED_EDGE('',*,*,#983,.F.);
#1279=ORIENTED_EDGE('',*,*,#1012,.F.);
#1280=ORIENTED_EDGE('',*,*,#977,.T.);
#1281=ORIENTED_EDGE('',*,*,#1011,.T.);
#1282=ORIENTED_EDGE('',*,*,#986,.F.);
#1283=ORIENTED_EDGE('',*,*,#1013,.F.);
#1284=ORIENTED_EDGE('',*,*,#970,.T.);
#1285=ORIENTED_EDGE('',*,*,#1012,.T.);
#1286=ORIENTED_EDGE('',*,*,#973,.F.);
#1287=ORIENTED_EDGE('',*,*,#944,.F.);
#1288=ORIENTED_EDGE('',*,*,#967,.T.);
#1289=ORIENTED_EDGE('',*,*,#1013,.T.);
#1290=ORIENTED_EDGE('',*,*,#975,.T.);
#1291=ORIENTED_EDGE('',*,*,#1014,.F.);
#1292=ORIENTED_EDGE('',*,*,#969,.F.);
#1293=ORIENTED_EDGE('',*,*,#929,.T.);
#1294=ORIENTED_EDGE('',*,*,#987,.T.);
#1295=ORIENTED_EDGE('',*,*,#1015,.F.);
#1296=ORIENTED_EDGE('',*,*,#971,.F.);
#1297=ORIENTED_EDGE('',*,*,#1014,.T.);
#1298=ORIENTED_EDGE('',*,*,#985,.T.);
#1299=ORIENTED_EDGE('',*,*,#1016,.F.);
#1300=ORIENTED_EDGE('',*,*,#978,.F.);
#1301=ORIENTED_EDGE('',*,*,#1015,.T.);
#1302=ORIENTED_EDGE('',*,*,#999,.T.);
#1303=ORIENTED_EDGE('',*,*,#1017,.F.);
#1304=ORIENTED_EDGE('',*,*,#980,.F.);
#1305=ORIENTED_EDGE('',*,*,#1016,.T.);
#1306=ORIENTED_EDGE('',*,*,#997,.T.);
#1307=ORIENTED_EDGE('',*,*,#1018,.F.);
#1308=ORIENTED_EDGE('',*,*,#990,.F.);
#1309=ORIENTED_EDGE('',*,*,#1017,.T.);
#1310=ORIENTED_EDGE('',*,*,#1007,.T.);
#1311=ORIENTED_EDGE('',*,*,#1019,.F.);
#1312=ORIENTED_EDGE('',*,*,#992,.F.);
#1313=ORIENTED_EDGE('',*,*,#1018,.T.);
#1314=ORIENTED_EDGE('',*,*,#1005,.T.);
#1315=ORIENTED_EDGE('',*,*,#927,.F.);
#1316=ORIENTED_EDGE('',*,*,#1001,.F.);
#1317=ORIENTED_EDGE('',*,*,#1019,.T.);
#1318=ORIENTED_EDGE('',*,*,#1020,.F.);
#1319=ORIENTED_EDGE('',*,*,#1021,.F.);
#1320=ORIENTED_EDGE('',*,*,#965,.F.);
#1321=ORIENTED_EDGE('',*,*,#930,.T.);
#1322=ORIENTED_EDGE('',*,*,#968,.T.);
#1323=ORIENTED_EDGE('',*,*,#943,.F.);
#1324=ORIENTED_EDGE('',*,*,#938,.T.);
#1325=ORIENTED_EDGE('',*,*,#1022,.F.);
#1326=ORIENTED_EDGE('',*,*,#1023,.F.);
#1327=ORIENTED_EDGE('',*,*,#958,.T.);
#1328=ORIENTED_EDGE('',*,*,#924,.F.);
#1329=ORIENTED_EDGE('',*,*,#1004,.T.);
#1330=ORIENTED_EDGE('',*,*,#936,.F.);
#1331=ORIENTED_EDGE('',*,*,#960,.F.);
#1332=ORIENTED_EDGE('',*,*,#1024,.T.);
#1333=ORIENTED_EDGE('',*,*,#1025,.T.);
#1334=ORIENTED_EDGE('',*,*,#937,.T.);
#1335=ORIENTED_EDGE('',*,*,#1025,.F.);
#1336=ORIENTED_EDGE('',*,*,#1026,.F.);
#1337=ORIENTED_EDGE('',*,*,#1022,.T.);
#1338=ORIENTED_EDGE('',*,*,#1023,.T.);
#1339=ORIENTED_EDGE('',*,*,#1026,.T.);
#1340=ORIENTED_EDGE('',*,*,#1024,.F.);
#1341=ORIENTED_EDGE('',*,*,#959,.F.);
#1342=ORIENTED_EDGE('',*,*,#900,.T.);
#1343=ORIENTED_EDGE('',*,*,#941,.F.);
#1344=ORIENTED_EDGE('',*,*,#962,.F.);
#1345=ORIENTED_EDGE('',*,*,#1027,.T.);
#1346=ORIENTED_EDGE('',*,*,#1028,.T.);
#1347=ORIENTED_EDGE('',*,*,#942,.T.);
#1348=ORIENTED_EDGE('',*,*,#1028,.F.);
#1349=ORIENTED_EDGE('',*,*,#1029,.F.);
#1350=ORIENTED_EDGE('',*,*,#1020,.T.);
#1351=ORIENTED_EDGE('',*,*,#1021,.T.);
#1352=ORIENTED_EDGE('',*,*,#1029,.T.);
#1353=ORIENTED_EDGE('',*,*,#1027,.F.);
#1354=ORIENTED_EDGE('',*,*,#961,.T.);
#1355=ORIENTED_EDGE('',*,*,#903,.T.);
#1356=ORIENTED_EDGE('',*,*,#946,.F.);
#1357=ORIENTED_EDGE('',*,*,#949,.F.);
#1358=ORIENTED_EDGE('',*,*,#1030,.T.);
#1359=ORIENTED_EDGE('',*,*,#1031,.T.);
#1360=ORIENTED_EDGE('',*,*,#947,.T.);
#1361=ORIENTED_EDGE('',*,*,#1031,.F.);
#1362=ORIENTED_EDGE('',*,*,#1032,.F.);
#1363=ORIENTED_EDGE('',*,*,#963,.T.);
#1364=ORIENTED_EDGE('',*,*,#964,.T.);
#1365=ORIENTED_EDGE('',*,*,#1032,.T.);
#1366=ORIENTED_EDGE('',*,*,#1030,.F.);
#1367=ORIENTED_EDGE('',*,*,#948,.T.);
#1368=ORIENTED_EDGE('',*,*,#906,.F.);
#1369=ORIENTED_EDGE('',*,*,#933,.F.);
#1370=ORIENTED_EDGE('',*,*,#953,.F.);
#1371=ORIENTED_EDGE('',*,*,#1033,.T.);
#1372=ORIENTED_EDGE('',*,*,#1034,.T.);
#1373=ORIENTED_EDGE('',*,*,#934,.T.);
#1374=ORIENTED_EDGE('',*,*,#1034,.F.);
#1375=ORIENTED_EDGE('',*,*,#1035,.F.);
#1376=ORIENTED_EDGE('',*,*,#956,.T.);
#1377=ORIENTED_EDGE('',*,*,#952,.F.);
#1378=ORIENTED_EDGE('',*,*,#957,.T.);
#1379=ORIENTED_EDGE('',*,*,#1035,.T.);
#1380=ORIENTED_EDGE('',*,*,#1033,.F.);
#1381=ORIENTED_EDGE('',*,*,#909,.F.);
#1382=ORIENTED_EDGE('',*,*,#1036,.T.);
#1383=ORIENTED_EDGE('',*,*,#1037,.T.);
#1384=ORIENTED_EDGE('',*,*,#1038,.T.);
#1385=ORIENTED_EDGE('',*,*,#1037,.F.);
#1386=ORIENTED_EDGE('',*,*,#1039,.T.);
#1387=ORIENTED_EDGE('',*,*,#1040,.T.);
#1388=ORIENTED_EDGE('',*,*,#1041,.T.);
#1389=ORIENTED_EDGE('',*,*,#1040,.F.);
#1390=ORIENTED_EDGE('',*,*,#1042,.T.);
#1391=ORIENTED_EDGE('',*,*,#1043,.F.);
#1392=ORIENTED_EDGE('',*,*,#1044,.F.);
#1393=ORIENTED_EDGE('',*,*,#1045,.T.);
#1394=ORIENTED_EDGE('',*,*,#1038,.F.);
#1395=ORIENTED_EDGE('',*,*,#1041,.F.);
#1396=ORIENTED_EDGE('',*,*,#1046,.T.);
#1397=ORIENTED_EDGE('',*,*,#1047,.F.);
#1398=ORIENTED_EDGE('',*,*,#1048,.F.);
#1399=ORIENTED_EDGE('',*,*,#1043,.T.);
#1400=ORIENTED_EDGE('',*,*,#1049,.T.);
#1401=ORIENTED_EDGE('',*,*,#1050,.F.);
#1402=ORIENTED_EDGE('',*,*,#1051,.F.);
#1403=ORIENTED_EDGE('',*,*,#1047,.T.);
#1404=ORIENTED_EDGE('',*,*,#1052,.F.);
#1405=ORIENTED_EDGE('',*,*,#1053,.F.);
#1406=ORIENTED_EDGE('',*,*,#1054,.T.);
#1407=ORIENTED_EDGE('',*,*,#1055,.T.);
#1408=ORIENTED_EDGE('',*,*,#1056,.F.);
#1409=ORIENTED_EDGE('',*,*,#1057,.F.);
#1410=ORIENTED_EDGE('',*,*,#1058,.T.);
#1411=ORIENTED_EDGE('',*,*,#1053,.T.);
#1412=ORIENTED_EDGE('',*,*,#1059,.F.);
#1413=ORIENTED_EDGE('',*,*,#1060,.F.);
#1414=ORIENTED_EDGE('',*,*,#1061,.T.);
#1415=ORIENTED_EDGE('',*,*,#1057,.T.);
#1416=ORIENTED_EDGE('',*,*,#1062,.F.);
#1417=ORIENTED_EDGE('',*,*,#1055,.F.);
#1418=ORIENTED_EDGE('',*,*,#1063,.T.);
#1419=ORIENTED_EDGE('',*,*,#1060,.T.);
#1420=ORIENTED_EDGE('',*,*,#1036,.F.);
#1421=ORIENTED_EDGE('',*,*,#1039,.F.);
#1422=ORIENTED_EDGE('',*,*,#1064,.T.);
#1423=ORIENTED_EDGE('',*,*,#1045,.F.);
#1424=ORIENTED_EDGE('',*,*,#1065,.F.);
#1425=ORIENTED_EDGE('',*,*,#1050,.T.);
#1426=ORIENTED_EDGE('',*,*,#1044,.T.);
#1427=ORIENTED_EDGE('',*,*,#1048,.T.);
#1428=ORIENTED_EDGE('',*,*,#1051,.T.);
#1429=ORIENTED_EDGE('',*,*,#1065,.T.);
#1430=ORIENTED_EDGE('',*,*,#1054,.F.);
#1431=ORIENTED_EDGE('',*,*,#1058,.F.);
#1432=ORIENTED_EDGE('',*,*,#1061,.F.);
#1433=ORIENTED_EDGE('',*,*,#1063,.F.);
#1434=ORIENTED_EDGE('',*,*,#1042,.F.);
#1435=ORIENTED_EDGE('',*,*,#1064,.F.);
#1436=ORIENTED_EDGE('',*,*,#1049,.F.);
#1437=ORIENTED_EDGE('',*,*,#1046,.F.);
#1438=ORIENTED_EDGE('',*,*,#1052,.T.);
#1439=ORIENTED_EDGE('',*,*,#1062,.T.);
#1440=ORIENTED_EDGE('',*,*,#1059,.T.);
#1441=ORIENTED_EDGE('',*,*,#1056,.T.);
#1442=ORIENTED_EDGE('',*,*,#1066,.T.);
#1443=ORIENTED_EDGE('',*,*,#1067,.F.);
#1444=ORIENTED_EDGE('',*,*,#1068,.F.);
#1445=ORIENTED_EDGE('',*,*,#1069,.T.);
#1446=ORIENTED_EDGE('',*,*,#1070,.T.);
#1447=ORIENTED_EDGE('',*,*,#1071,.F.);
#1448=ORIENTED_EDGE('',*,*,#1072,.F.);
#1449=ORIENTED_EDGE('',*,*,#1067,.T.);
#1450=ORIENTED_EDGE('',*,*,#1073,.T.);
#1451=ORIENTED_EDGE('',*,*,#1074,.F.);
#1452=ORIENTED_EDGE('',*,*,#1075,.F.);
#1453=ORIENTED_EDGE('',*,*,#1071,.T.);
#1454=ORIENTED_EDGE('',*,*,#1076,.T.);
#1455=ORIENTED_EDGE('',*,*,#1077,.F.);
#1456=ORIENTED_EDGE('',*,*,#1078,.F.);
#1457=ORIENTED_EDGE('',*,*,#1074,.T.);
#1458=ORIENTED_EDGE('',*,*,#1079,.T.);
#1459=ORIENTED_EDGE('',*,*,#1080,.F.);
#1460=ORIENTED_EDGE('',*,*,#1081,.F.);
#1461=ORIENTED_EDGE('',*,*,#1077,.T.);
#1462=ORIENTED_EDGE('',*,*,#1082,.T.);
#1463=ORIENTED_EDGE('',*,*,#1083,.F.);
#1464=ORIENTED_EDGE('',*,*,#1084,.F.);
#1465=ORIENTED_EDGE('',*,*,#1080,.T.);
#1466=ORIENTED_EDGE('',*,*,#1085,.T.);
#1467=ORIENTED_EDGE('',*,*,#1086,.F.);
#1468=ORIENTED_EDGE('',*,*,#1087,.F.);
#1469=ORIENTED_EDGE('',*,*,#1083,.T.);
#1470=ORIENTED_EDGE('',*,*,#1088,.T.);
#1471=ORIENTED_EDGE('',*,*,#1069,.F.);
#1472=ORIENTED_EDGE('',*,*,#1089,.F.);
#1473=ORIENTED_EDGE('',*,*,#1086,.T.);
#1474=ORIENTED_EDGE('',*,*,#1068,.T.);
#1475=ORIENTED_EDGE('',*,*,#1072,.T.);
#1476=ORIENTED_EDGE('',*,*,#1075,.T.);
#1477=ORIENTED_EDGE('',*,*,#1078,.T.);
#1478=ORIENTED_EDGE('',*,*,#1081,.T.);
#1479=ORIENTED_EDGE('',*,*,#1084,.T.);
#1480=ORIENTED_EDGE('',*,*,#1087,.T.);
#1481=ORIENTED_EDGE('',*,*,#1089,.T.);
#1482=ORIENTED_EDGE('',*,*,#1066,.F.);
#1483=ORIENTED_EDGE('',*,*,#1088,.F.);
#1484=ORIENTED_EDGE('',*,*,#1085,.F.);
#1485=ORIENTED_EDGE('',*,*,#1082,.F.);
#1486=ORIENTED_EDGE('',*,*,#1079,.F.);
#1487=ORIENTED_EDGE('',*,*,#1076,.F.);
#1488=ORIENTED_EDGE('',*,*,#1073,.F.);
#1489=ORIENTED_EDGE('',*,*,#1070,.F.);
#1490=ORIENTED_EDGE('',*,*,#1090,.T.);
#1491=ORIENTED_EDGE('',*,*,#1091,.F.);
#1492=ORIENTED_EDGE('',*,*,#1092,.F.);
#1493=ORIENTED_EDGE('',*,*,#1093,.T.);
#1494=ORIENTED_EDGE('',*,*,#1094,.T.);
#1495=ORIENTED_EDGE('',*,*,#1095,.F.);
#1496=ORIENTED_EDGE('',*,*,#1096,.F.);
#1497=ORIENTED_EDGE('',*,*,#1091,.T.);
#1498=ORIENTED_EDGE('',*,*,#1097,.T.);
#1499=ORIENTED_EDGE('',*,*,#1098,.F.);
#1500=ORIENTED_EDGE('',*,*,#1099,.F.);
#1501=ORIENTED_EDGE('',*,*,#1095,.T.);
#1502=ORIENTED_EDGE('',*,*,#1100,.T.);
#1503=ORIENTED_EDGE('',*,*,#1093,.F.);
#1504=ORIENTED_EDGE('',*,*,#1101,.F.);
#1505=ORIENTED_EDGE('',*,*,#1098,.T.);
#1506=ORIENTED_EDGE('',*,*,#1092,.T.);
#1507=ORIENTED_EDGE('',*,*,#1096,.T.);
#1508=ORIENTED_EDGE('',*,*,#1099,.T.);
#1509=ORIENTED_EDGE('',*,*,#1101,.T.);
#1510=ORIENTED_EDGE('',*,*,#1090,.F.);
#1511=ORIENTED_EDGE('',*,*,#1100,.F.);
#1512=ORIENTED_EDGE('',*,*,#1097,.F.);
#1513=ORIENTED_EDGE('',*,*,#1094,.F.);
#1514=ORIENTED_EDGE('',*,*,#1102,.F.);
#1515=ORIENTED_EDGE('',*,*,#1103,.T.);
#1516=ORIENTED_EDGE('',*,*,#1104,.F.);
#1517=ORIENTED_EDGE('',*,*,#1103,.F.);
#1518=ORIENTED_EDGE('',*,*,#1105,.T.);
#1519=ORIENTED_EDGE('',*,*,#1106,.T.);
#1520=ORIENTED_EDGE('',*,*,#1102,.T.);
#1521=ORIENTED_EDGE('',*,*,#1106,.F.);
#1522=ORIENTED_EDGE('',*,*,#1107,.T.);
#1523=ORIENTED_EDGE('',*,*,#1108,.T.);
#1524=ORIENTED_EDGE('',*,*,#1109,.F.);
#1525=ORIENTED_EDGE('',*,*,#1108,.F.);
#1526=ORIENTED_EDGE('',*,*,#1109,.T.);
#1527=ORIENTED_EDGE('',*,*,#1105,.F.);
#1528=ORIENTED_EDGE('',*,*,#1107,.F.);
#1529=ORIENTED_EDGE('',*,*,#1104,.T.);
#1530=CYLINDRICAL_SURFACE('',#1704,6.99999999999993);
#1531=CYLINDRICAL_SURFACE('',#1707,7.00000000000001);
#1532=CYLINDRICAL_SURFACE('',#1710,6.99999999999996);
#1533=CYLINDRICAL_SURFACE('',#1713,6.9999999999999);
#1534=CYLINDRICAL_SURFACE('',#1716,21.5);
#1535=CYLINDRICAL_SURFACE('',#1719,21.5);
#1536=CYLINDRICAL_SURFACE('',#1722,21.5);
#1537=CYLINDRICAL_SURFACE('',#1725,21.5);
#1538=CYLINDRICAL_SURFACE('',#1766,7.34999999999997);
#1539=CYLINDRICAL_SURFACE('',#1768,1.);
#1540=CYLINDRICAL_SURFACE('',#1770,1.);
#1541=CYLINDRICAL_SURFACE('',#1772,7.35);
#1542=CYLINDRICAL_SURFACE('',#1773,1.);
#1543=CYLINDRICAL_SURFACE('',#1775,7.35000000000002);
#1544=CYLINDRICAL_SURFACE('',#1777,7.35000000000002);
#1545=CYLINDRICAL_SURFACE('',#1779,1.);
#1546=CYLINDRICAL_SURFACE('',#1795,21.5000000000002);
#1547=CYLINDRICAL_SURFACE('',#1798,21.5000000000002);
#1548=CYLINDRICAL_SURFACE('',#1833,17.6799999999998);
#1549=CYLINDRICAL_SURFACE('',#1835,21.0799999999997);
#1550=ADVANCED_FACE('',(#186),#1530,.F.);
#1551=ADVANCED_FACE('',(#187),#1531,.F.);
#1552=ADVANCED_FACE('',(#188),#1532,.F.);
#1553=ADVANCED_FACE('',(#189),#1533,.F.);
#1554=ADVANCED_FACE('',(#190),#1534,.F.);
#1555=ADVANCED_FACE('',(#191),#1535,.F.);
#1556=ADVANCED_FACE('',(#192),#1536,.F.);
#1557=ADVANCED_FACE('',(#193),#1537,.F.);
#1558=ADVANCED_FACE('',(#194,#92,#93,#94,#95),#116,.F.);
#1559=ADVANCED_FACE('',(#195,#96,#97,#98,#99),#117,.F.);
#1560=ADVANCED_FACE('',(#196,#100,#101),#118,.T.);
#1561=ADVANCED_FACE('',(#197,#102,#103),#119,.T.);
#1562=ADVANCED_FACE('',(#198),#120,.T.);
#1563=ADVANCED_FACE('',(#199),#121,.T.);
#1564=ADVANCED_FACE('',(#200),#122,.T.);
#1565=ADVANCED_FACE('',(#201),#123,.T.);
#1566=ADVANCED_FACE('',(#202),#124,.T.);
#1567=ADVANCED_FACE('',(#203),#125,.T.);
#1568=ADVANCED_FACE('',(#204),#126,.T.);
#1569=ADVANCED_FACE('',(#205),#127,.T.);
#1570=ADVANCED_FACE('',(#206),#128,.T.);
#1571=ADVANCED_FACE('',(#207),#129,.T.);
#1572=ADVANCED_FACE('',(#208),#130,.T.);
#1573=ADVANCED_FACE('',(#209),#131,.T.);
#1574=ADVANCED_FACE('',(#210),#132,.T.);
#1575=ADVANCED_FACE('',(#211),#133,.T.);
#1576=ADVANCED_FACE('',(#212),#134,.T.);
#1577=ADVANCED_FACE('',(#213),#135,.T.);
#1578=ADVANCED_FACE('',(#214),#136,.T.);
#1579=ADVANCED_FACE('',(#215),#137,.T.);
#1580=ADVANCED_FACE('',(#216),#1538,.T.);
#1581=ADVANCED_FACE('',(#217),#138,.T.);
#1582=ADVANCED_FACE('',(#218),#1539,.F.);
#1583=ADVANCED_FACE('',(#219),#139,.T.);
#1584=ADVANCED_FACE('',(#220),#1540,.F.);
#1585=ADVANCED_FACE('',(#221),#140,.T.);
#1586=ADVANCED_FACE('',(#222),#1541,.T.);
#1587=ADVANCED_FACE('',(#223),#1542,.F.);
#1588=ADVANCED_FACE('',(#224),#141,.F.);
#1589=ADVANCED_FACE('',(#225),#1543,.T.);
#1590=ADVANCED_FACE('',(#226),#142,.F.);
#1591=ADVANCED_FACE('',(#227),#1544,.T.);
#1592=ADVANCED_FACE('',(#228),#143,.F.);
#1593=ADVANCED_FACE('',(#229),#1545,.F.);
#1594=ADVANCED_FACE('',(#230),#144,.T.);
#1595=ADVANCED_FACE('',(#231),#145,.F.);
#1596=ADVANCED_FACE('',(#232),#146,.T.);
#1597=ADVANCED_FACE('',(#233),#147,.F.);
#1598=ADVANCED_FACE('',(#234,#104),#148,.T.);
#1599=ADVANCED_FACE('',(#235),#149,.T.);
#1600=ADVANCED_FACE('',(#236),#150,.F.);
#1601=ADVANCED_FACE('',(#237,#105),#151,.T.);
#1602=ADVANCED_FACE('',(#238),#152,.T.);
#1603=ADVANCED_FACE('',(#239),#153,.F.);
#1604=ADVANCED_FACE('',(#240,#106),#154,.T.);
#1605=ADVANCED_FACE('',(#241),#155,.T.);
#1606=ADVANCED_FACE('',(#242),#156,.F.);
#1607=ADVANCED_FACE('',(#243,#107),#157,.T.);
#1608=ADVANCED_FACE('',(#244),#1546,.F.);
#1609=ADVANCED_FACE('',(#245),#1547,.F.);
#1610=ADVANCED_FACE('',(#246,#108,#109),#158,.F.);
#1611=ADVANCED_FACE('',(#247),#159,.F.);
#1612=ADVANCED_FACE('',(#248),#160,.F.);
#1613=ADVANCED_FACE('',(#249),#161,.T.);
#1614=ADVANCED_FACE('',(#250),#162,.T.);
#1615=ADVANCED_FACE('',(#251),#163,.T.);
#1616=ADVANCED_FACE('',(#252,#110,#111),#164,.T.);
#1617=ADVANCED_FACE('',(#253),#165,.F.);
#1618=ADVANCED_FACE('',(#254,#112),#166,.T.);
#1619=ADVANCED_FACE('',(#255,#113),#167,.F.);
#1620=ADVANCED_FACE('',(#256),#168,.F.);
#1621=ADVANCED_FACE('',(#257),#169,.F.);
#1622=ADVANCED_FACE('',(#258),#170,.F.);
#1623=ADVANCED_FACE('',(#259),#171,.F.);
#1624=ADVANCED_FACE('',(#260),#172,.F.);
#1625=ADVANCED_FACE('',(#261),#173,.F.);
#1626=ADVANCED_FACE('',(#262),#174,.F.);
#1627=ADVANCED_FACE('',(#263),#175,.F.);
#1628=ADVANCED_FACE('',(#264),#176,.F.);
#1629=ADVANCED_FACE('',(#265),#177,.T.);
#1630=ADVANCED_FACE('',(#266),#178,.F.);
#1631=ADVANCED_FACE('',(#267),#179,.F.);
#1632=ADVANCED_FACE('',(#268),#180,.F.);
#1633=ADVANCED_FACE('',(#269),#181,.F.);
#1634=ADVANCED_FACE('',(#270),#182,.F.);
#1635=ADVANCED_FACE('',(#271),#183,.T.);
#1636=ADVANCED_FACE('',(#272),#71,.F.);
#1637=ADVANCED_FACE('',(#273),#1548,.F.);
#1638=ADVANCED_FACE('',(#274),#1549,.T.);
#1639=ADVANCED_FACE('',(#275,#114),#184,.T.);
#1640=ADVANCED_FACE('',(#276,#115),#185,.F.);
#1641=CLOSED_SHELL('',(#1550,#1551,#1552,#1553,#1554,#1555,#1556,#1557,
#1558,#1559,#1560,#1561,#1562,#1563,#1564,#1565,#1566,#1567,#1568,#1569,
#1570,#1571,#1572,#1573,#1574,#1575,#1576,#1577,#1578,#1579,#1580,#1581,
#1582,#1583,#1584,#1585,#1586,#1587,#1588,#1589,#1590,#1591,#1592,#1593,
#1594,#1595,#1596,#1597,#1598,#1599,#1600,#1601,#1602,#1603,#1604,#1605,
#1606,#1607));
#1642=CLOSED_SHELL('',(#1608,#1609,#1610,#1611,#1612,#1613,#1614,#1615,
#1616,#1617,#1618,#1619));
#1643=CLOSED_SHELL('',(#1620,#1621,#1622,#1623,#1624,#1625,#1626,#1627,
#1628,#1629));
#1644=CLOSED_SHELL('',(#1630,#1631,#1632,#1633,#1634,#1635));
#1645=CLOSED_SHELL('',(#1636,#1637,#1638,#1639,#1640));
#1646=DERIVED_UNIT_ELEMENT(#1656,1.);
#1647=DERIVED_UNIT_ELEMENT(#2796,-3.);
#1648=DERIVED_UNIT_ELEMENT(#1656,1.);
#1649=DERIVED_UNIT_ELEMENT(#2796,-3.);
#1650=DERIVED_UNIT_ELEMENT(#1656,1.);
#1651=DERIVED_UNIT_ELEMENT(#2796,-3.);
#1652=DERIVED_UNIT_ELEMENT(#1656,1.);
#1653=DERIVED_UNIT_ELEMENT(#2796,-3.);
#1654=DERIVED_UNIT_ELEMENT(#1656,1.);
#1655=DERIVED_UNIT_ELEMENT(#2796,-3.);
#1656=(
MASS_UNIT()
NAMED_UNIT(*)
SI_UNIT(.KILO.,.GRAM.)
);
#1657=DERIVED_UNIT((#1646,#1647));
#1658=DERIVED_UNIT((#1648,#1649));
#1659=DERIVED_UNIT((#1650,#1651));
#1660=DERIVED_UNIT((#1652,#1653));
#1661=DERIVED_UNIT((#1654,#1655));
#1662=MEASURE_REPRESENTATION_ITEM('density measure',
POSITIVE_RATIO_MEASURE(7850.),#1657);
#1663=MEASURE_REPRESENTATION_ITEM('density measure',
POSITIVE_RATIO_MEASURE(7850.),#1658);
#1664=MEASURE_REPRESENTATION_ITEM('density measure',
POSITIVE_RATIO_MEASURE(7850.),#1659);
#1665=MEASURE_REPRESENTATION_ITEM('density measure',
POSITIVE_RATIO_MEASURE(7850.),#1660);
#1666=MEASURE_REPRESENTATION_ITEM('density measure',
POSITIVE_RATIO_MEASURE(7850.),#1661);
#1667=PROPERTY_DEFINITION_REPRESENTATION(#1692,#1677);
#1668=PROPERTY_DEFINITION_REPRESENTATION(#1693,#1678);
#1669=PROPERTY_DEFINITION_REPRESENTATION(#1694,#1679);
#1670=PROPERTY_DEFINITION_REPRESENTATION(#1695,#1680);
#1671=PROPERTY_DEFINITION_REPRESENTATION(#1696,#1681);
#1672=PROPERTY_DEFINITION_REPRESENTATION(#1697,#1682);
#1673=PROPERTY_DEFINITION_REPRESENTATION(#1698,#1683);
#1674=PROPERTY_DEFINITION_REPRESENTATION(#1699,#1684);
#1675=PROPERTY_DEFINITION_REPRESENTATION(#1700,#1685);
#1676=PROPERTY_DEFINITION_REPRESENTATION(#1701,#1686);
#1677=REPRESENTATION('material name',(#1687),#2789);
#1678=REPRESENTATION('density',(#1662),#2789);
#1679=REPRESENTATION('material name',(#1688),#2790);
#1680=REPRESENTATION('density',(#1663),#2790);
#1681=REPRESENTATION('material name',(#1689),#2791);
#1682=REPRESENTATION('density',(#1664),#2791);
#1683=REPRESENTATION('material name',(#1690),#2792);
#1684=REPRESENTATION('density',(#1665),#2792);
#1685=REPRESENTATION('material name',(#1691),#2793);
#1686=REPRESENTATION('density',(#1666),#2793);
#1687=DESCRIPTIVE_REPRESENTATION_ITEM('Steel','Steel');
#1688=DESCRIPTIVE_REPRESENTATION_ITEM('Steel','Steel');
#1689=DESCRIPTIVE_REPRESENTATION_ITEM('Steel','Steel');
#1690=DESCRIPTIVE_REPRESENTATION_ITEM('Steel','Steel');
#1691=DESCRIPTIVE_REPRESENTATION_ITEM('Steel','Steel');
#1692=PROPERTY_DEFINITION('material property','material name',#2834);
#1693=PROPERTY_DEFINITION('material property','density of part',#2834);
#1694=PROPERTY_DEFINITION('material property','material name',#2835);
#1695=PROPERTY_DEFINITION('material property','density of part',#2835);
#1696=PROPERTY_DEFINITION('material property','material name',#2836);
#1697=PROPERTY_DEFINITION('material property','density of part',#2836);
#1698=PROPERTY_DEFINITION('material property','material name',#2837);
#1699=PROPERTY_DEFINITION('material property','density of part',#2837);
#1700=PROPERTY_DEFINITION('material property','material name',#2838);
#1701=PROPERTY_DEFINITION('material property','density of part',#2838);
#1702=AXIS2_PLACEMENT_3D('',#2330,#1855,#1856);
#1703=AXIS2_PLACEMENT_3D('',#2331,#1857,#1858);
#1704=AXIS2_PLACEMENT_3D('',#2332,#1859,#1860);
#1705=AXIS2_PLACEMENT_3D('',#2334,#1861,#1862);
#1706=AXIS2_PLACEMENT_3D('',#2337,#1864,#1865);
#1707=AXIS2_PLACEMENT_3D('',#2338,#1866,#1867);
#1708=AXIS2_PLACEMENT_3D('',#2340,#1868,#1869);
#1709=AXIS2_PLACEMENT_3D('',#2343,#1871,#1872);
#1710=AXIS2_PLACEMENT_3D('',#2344,#1873,#1874);
#1711=AXIS2_PLACEMENT_3D('',#2346,#1875,#1876);
#1712=AXIS2_PLACEMENT_3D('',#2349,#1878,#1879);
#1713=AXIS2_PLACEMENT_3D('',#2350,#1880,#1881);
#1714=AXIS2_PLACEMENT_3D('',#2352,#1882,#1883);
#1715=AXIS2_PLACEMENT_3D('',#2355,#1885,#1886);
#1716=AXIS2_PLACEMENT_3D('',#2356,#1887,#1888);
#1717=AXIS2_PLACEMENT_3D('',#2358,#1889,#1890);
#1718=AXIS2_PLACEMENT_3D('',#2361,#1892,#1893);
#1719=AXIS2_PLACEMENT_3D('',#2362,#1894,#1895);
#1720=AXIS2_PLACEMENT_3D('',#2364,#1896,#1897);
#1721=AXIS2_PLACEMENT_3D('',#2367,#1899,#1900);
#1722=AXIS2_PLACEMENT_3D('',#2368,#1901,#1902);
#1723=AXIS2_PLACEMENT_3D('',#2370,#1903,#1904);
#1724=AXIS2_PLACEMENT_3D('',#2373,#1906,#1907);
#1725=AXIS2_PLACEMENT_3D('',#2374,#1908,#1909);
#1726=AXIS2_PLACEMENT_3D('',#2376,#1910,#1911);
#1727=AXIS2_PLACEMENT_3D('',#2379,#1913,#1914);
#1728=AXIS2_PLACEMENT_3D('',#2380,#1915,#1916);
#1729=AXIS2_PLACEMENT_3D('',#2389,#1921,#1922);
#1730=AXIS2_PLACEMENT_3D('',#2398,#1927,#1928);
#1731=AXIS2_PLACEMENT_3D('',#2415,#1937,#1938);
#1732=AXIS2_PLACEMENT_3D('',#2432,#1947,#1948);
#1733=AXIS2_PLACEMENT_3D('',#2439,#1953,#1954);
#1734=AXIS2_PLACEMENT_3D('',#2446,#1959,#1960);
#1735=AXIS2_PLACEMENT_3D('',#2455,#1966,#1967);
#1736=AXIS2_PLACEMENT_3D('',#2464,#1973,#1974);
#1737=AXIS2_PLACEMENT_3D('',#2468,#1976,#1977);
#1738=AXIS2_PLACEMENT_3D('',#2470,#1979,#1980);
#1739=AXIS2_PLACEMENT_3D('',#2471,#1981,#1982);
#1740=AXIS2_PLACEMENT_3D('',#2477,#1986,#1987);
#1741=AXIS2_PLACEMENT_3D('',#2479,#1988,#1989);
#1742=AXIS2_PLACEMENT_3D('',#2482,#1991,#1992);
#1743=AXIS2_PLACEMENT_3D('',#2483,#1993,#1994);
#1744=AXIS2_PLACEMENT_3D('',#2487,#1996,#1997);
#1745=AXIS2_PLACEMENT_3D('',#2488,#1998,#1999);
#1746=AXIS2_PLACEMENT_3D('',#2489,#2000,#2001);
#1747=AXIS2_PLACEMENT_3D('',#2495,#2005,#2006);
#1748=AXIS2_PLACEMENT_3D('',#2500,#2008,#2009);
#1749=AXIS2_PLACEMENT_3D('',#2503,#2011,#2012);
#1750=AXIS2_PLACEMENT_3D('',#2504,#2013,#2014);
#1751=AXIS2_PLACEMENT_3D('',#2507,#2017,#2018);
#1752=AXIS2_PLACEMENT_3D('',#2511,#2020,#2021);
#1753=AXIS2_PLACEMENT_3D('',#2512,#2022,#2023);
#1754=AXIS2_PLACEMENT_3D('',#2513,#2024,#2025);
#1755=AXIS2_PLACEMENT_3D('',#2519,#2029,#2030);
#1756=AXIS2_PLACEMENT_3D('',#2524,#2032,#2033);
#1757=AXIS2_PLACEMENT_3D('',#2527,#2035,#2036);
#1758=AXIS2_PLACEMENT_3D('',#2528,#2037,#2038);
#1759=AXIS2_PLACEMENT_3D('',#2531,#2041,#2042);
#1760=AXIS2_PLACEMENT_3D('',#2532,#2043,#2044);
#1761=AXIS2_PLACEMENT_3D('',#2533,#2045,#2046);
#1762=AXIS2_PLACEMENT_3D('',#2534,#2047,#2048);
#1763=AXIS2_PLACEMENT_3D('',#2538,#2050,#2051);
#1764=AXIS2_PLACEMENT_3D('',#2540,#2053,#2054);
#1765=AXIS2_PLACEMENT_3D('',#2541,#2055,#2056);
#1766=AXIS2_PLACEMENT_3D('',#2544,#2059,#2060);
#1767=AXIS2_PLACEMENT_3D('',#2546,#2062,#2063);
#1768=AXIS2_PLACEMENT_3D('',#2548,#2065,#2066);
#1769=AXIS2_PLACEMENT_3D('',#2550,#2068,#2069);
#1770=AXIS2_PLACEMENT_3D('',#2552,#2071,#2072);
#1771=AXIS2_PLACEMENT_3D('',#2554,#2074,#2075);
#1772=AXIS2_PLACEMENT_3D('',#2556,#2077,#2078);
#1773=AXIS2_PLACEMENT_3D('',#2557,#2079,#2080);
#1774=AXIS2_PLACEMENT_3D('',#2559,#2082,#2083);
#1775=AXIS2_PLACEMENT_3D('',#2561,#2085,#2086);
#1776=AXIS2_PLACEMENT_3D('',#2563,#2088,#2089);
#1777=AXIS2_PLACEMENT_3D('',#2565,#2091,#2092);
#1778=AXIS2_PLACEMENT_3D('',#2567,#2094,#2095);
#1779=AXIS2_PLACEMENT_3D('',#2569,#2097,#2098);
#1780=AXIS2_PLACEMENT_3D('',#2570,#2099,#2100);
#1781=AXIS2_PLACEMENT_3D('',#2574,#2103,#2104);
#1782=AXIS2_PLACEMENT_3D('',#2578,#2107,#2108);
#1783=AXIS2_PLACEMENT_3D('',#2582,#2111,#2112);
#1784=AXIS2_PLACEMENT_3D('',#2584,#2114,#2115);
#1785=AXIS2_PLACEMENT_3D('',#2585,#2116,#2117);
#1786=AXIS2_PLACEMENT_3D('',#2589,#2120,#2121);
#1787=AXIS2_PLACEMENT_3D('',#2591,#2123,#2124);
#1788=AXIS2_PLACEMENT_3D('',#2592,#2125,#2126);
#1789=AXIS2_PLACEMENT_3D('',#2596,#2129,#2130);
#1790=AXIS2_PLACEMENT_3D('',#2598,#2132,#2133);
#1791=AXIS2_PLACEMENT_3D('',#2599,#2134,#2135);
#1792=AXIS2_PLACEMENT_3D('',#2603,#2138,#2139);
#1793=AXIS2_PLACEMENT_3D('',#2605,#2141,#2142);
#1794=AXIS2_PLACEMENT_3D('',#2606,#2143,#2144);
#1795=AXIS2_PLACEMENT_3D('',#2607,#2145,#2146);
#1796=AXIS2_PLACEMENT_3D('',#2609,#2147,#2148);
#1797=AXIS2_PLACEMENT_3D('',#2612,#2150,#2151);
#1798=AXIS2_PLACEMENT_3D('',#2613,#2152,#2153);
#1799=AXIS2_PLACEMENT_3D('',#2615,#2154,#2155);
#1800=AXIS2_PLACEMENT_3D('',#2618,#2157,#2158);
#1801=AXIS2_PLACEMENT_3D('',#2619,#2159,#2160);
#1802=AXIS2_PLACEMENT_3D('',#2628,#2165,#2166);
#1803=AXIS2_PLACEMENT_3D('',#2634,#2170,#2171);
#1804=AXIS2_PLACEMENT_3D('',#2640,#2175,#2176);
#1805=AXIS2_PLACEMENT_3D('',#2649,#2181,#2182);
#1806=AXIS2_PLACEMENT_3D('',#2655,#2186,#2187);
#1807=AXIS2_PLACEMENT_3D('',#2661,#2191,#2192);
#1808=AXIS2_PLACEMENT_3D('',#2664,#2195,#2196);
#1809=AXIS2_PLACEMENT_3D('',#2667,#2199,#2200);
#1810=AXIS2_PLACEMENT_3D('',#2668,#2201,#2202);
#1811=AXIS2_PLACEMENT_3D('',#2669,#2203,#2204);
#1812=AXIS2_PLACEMENT_3D('',#2670,#2205,#2206);
#1813=AXIS2_PLACEMENT_3D('',#2679,#2211,#2212);
#1814=AXIS2_PLACEMENT_3D('',#2685,#2216,#2217);
#1815=AXIS2_PLACEMENT_3D('',#2691,#2221,#2222);
#1816=AXIS2_PLACEMENT_3D('',#2697,#2226,#2227);
#1817=AXIS2_PLACEMENT_3D('',#2703,#2231,#2232);
#1818=AXIS2_PLACEMENT_3D('',#2709,#2236,#2237);
#1819=AXIS2_PLACEMENT_3D('',#2715,#2241,#2242);
#1820=AXIS2_PLACEMENT_3D('',#2718,#2245,#2246);
#1821=AXIS2_PLACEMENT_3D('',#2719,#2247,#2248);
#1822=AXIS2_PLACEMENT_3D('',#2720,#2249,#2250);
#1823=AXIS2_PLACEMENT_3D('',#2721,#2251,#2252);
#1824=AXIS2_PLACEMENT_3D('',#2730,#2257,#2258);
#1825=AXIS2_PLACEMENT_3D('',#2736,#2262,#2263);
#1826=AXIS2_PLACEMENT_3D('',#2742,#2267,#2268);
#1827=AXIS2_PLACEMENT_3D('',#2745,#2271,#2272);
#1828=AXIS2_PLACEMENT_3D('',#2746,#2273,#2274);
#1829=AXIS2_PLACEMENT_3D('',#2747,#2275,#2276);
#1830=AXIS2_PLACEMENT_3D('',#2748,#2277,#2278);
#1831=AXIS2_PLACEMENT_3D('',#2750,#2279,#2280);
#1832=AXIS2_PLACEMENT_3D('',#2753,#2282,#2283);
#1833=AXIS2_PLACEMENT_3D('',#2754,#2284,#2285);
#1834=AXIS2_PLACEMENT_3D('',#2756,#2286,#2287);
#1835=AXIS2_PLACEMENT_3D('',#2758,#2289,#2290);
#1836=AXIS2_PLACEMENT_3D('',#2760,#2291,#2292);
#1837=AXIS2_PLACEMENT_3D('',#2763,#2294,#2295);
#1838=AXIS2_PLACEMENT_3D('',#2764,#2296,#2297);
#1839=AXIS2_PLACEMENT_3D('',#2765,#2298,#2299);
#1840=AXIS2_PLACEMENT_3D('',#2766,#2300,#2301);
#1841=AXIS2_PLACEMENT_3D('',#2767,#2302,#2303);
#1842=AXIS2_PLACEMENT_3D('',#2768,#2304,#2305);
#1843=AXIS2_PLACEMENT_3D('',#2769,#2306,#2307);
#1844=AXIS2_PLACEMENT_3D('',#2770,#2308,#2309);
#1845=AXIS2_PLACEMENT_3D('',#2771,#2310,#2311);
#1846=AXIS2_PLACEMENT_3D('',#2772,#2312,#2313);
#1847=AXIS2_PLACEMENT_3D('',#2773,#2314,#2315);
#1848=AXIS2_PLACEMENT_3D('',#2774,#2316,#2317);
#1849=AXIS2_PLACEMENT_3D('',#2775,#2318,#2319);
#1850=AXIS2_PLACEMENT_3D('',#2776,#2320,#2321);
#1851=AXIS2_PLACEMENT_3D('',#2777,#2322,#2323);
#1852=AXIS2_PLACEMENT_3D('',#2778,#2324,#2325);
#1853=AXIS2_PLACEMENT_3D('',#2779,#2326,#2327);
#1854=AXIS2_PLACEMENT_3D('',#2780,#2328,#2329);
#1855=DIRECTION('axis',(0.,0.,1.));
#1856=DIRECTION('refdir',(1.,0.,0.));
#1857=DIRECTION('axis',(0.,0.,1.));
#1858=DIRECTION('refdir',(1.,0.,0.));
#1859=DIRECTION('center_axis',(0.,-1.,0.));
#1860=DIRECTION('ref_axis',(0.,0.,-1.));
#1861=DIRECTION('center_axis',(0.,-1.,0.));
#1862=DIRECTION('ref_axis',(0.,0.,1.));
#1863=DIRECTION('',(0.,-1.,0.));
#1864=DIRECTION('center_axis',(0.,-1.,0.));
#1865=DIRECTION('ref_axis',(0.,0.,1.));
#1866=DIRECTION('center_axis',(0.,-1.,0.));
#1867=DIRECTION('ref_axis',(0.,0.,-1.));
#1868=DIRECTION('center_axis',(0.,-1.,0.));
#1869=DIRECTION('ref_axis',(0.,0.,1.));
#1870=DIRECTION('',(0.,-1.,0.));
#1871=DIRECTION('center_axis',(0.,-1.,0.));
#1872=DIRECTION('ref_axis',(0.,0.,1.));
#1873=DIRECTION('center_axis',(0.,-1.,0.));
#1874=DIRECTION('ref_axis',(0.,0.,-1.));
#1875=DIRECTION('center_axis',(0.,1.,0.));
#1876=DIRECTION('ref_axis',(0.,0.,1.));
#1877=DIRECTION('',(0.,-1.,0.));
#1878=DIRECTION('center_axis',(0.,1.,0.));
#1879=DIRECTION('ref_axis',(0.,0.,1.));
#1880=DIRECTION('center_axis',(0.,-1.,0.));
#1881=DIRECTION('ref_axis',(0.,0.,-1.));
#1882=DIRECTION('center_axis',(0.,1.,0.));
#1883=DIRECTION('ref_axis',(0.,0.,1.));
#1884=DIRECTION('',(0.,-1.,0.));
#1885=DIRECTION('center_axis',(0.,1.,0.));
#1886=DIRECTION('ref_axis',(0.,0.,1.));
#1887=DIRECTION('center_axis',(0.,1.,0.));
#1888=DIRECTION('ref_axis',(0.,0.,1.));
#1889=DIRECTION('center_axis',(0.,-1.,0.));
#1890=DIRECTION('ref_axis',(0.,0.,1.));
#1891=DIRECTION('',(0.,1.,0.));
#1892=DIRECTION('center_axis',(0.,-1.,0.));
#1893=DIRECTION('ref_axis',(0.,0.,1.));
#1894=DIRECTION('center_axis',(0.,1.,0.));
#1895=DIRECTION('ref_axis',(0.,0.,1.));
#1896=DIRECTION('center_axis',(0.,1.,0.));
#1897=DIRECTION('ref_axis',(0.,0.,1.));
#1898=DIRECTION('',(0.,1.,0.));
#1899=DIRECTION('center_axis',(0.,1.,0.));
#1900=DIRECTION('ref_axis',(0.,0.,1.));
#1901=DIRECTION('center_axis',(0.,1.,0.));
#1902=DIRECTION('ref_axis',(0.,0.,1.));
#1903=DIRECTION('center_axis',(0.,-1.,0.));
#1904=DIRECTION('ref_axis',(0.,0.,1.));
#1905=DIRECTION('',(0.,1.,0.));
#1906=DIRECTION('center_axis',(0.,-1.,0.));
#1907=DIRECTION('ref_axis',(0.,0.,1.));
#1908=DIRECTION('center_axis',(0.,1.,0.));
#1909=DIRECTION('ref_axis',(0.,0.,1.));
#1910=DIRECTION('center_axis',(0.,1.,0.));
#1911=DIRECTION('ref_axis',(0.,0.,1.));
#1912=DIRECTION('',(0.,1.,0.));
#1913=DIRECTION('center_axis',(0.,1.,0.));
#1914=DIRECTION('ref_axis',(0.,0.,1.));
#1915=DIRECTION('center_axis',(0.,1.,0.));
#1916=DIRECTION('ref_axis',(0.,0.,1.));
#1917=DIRECTION('',(1.,0.,0.));
#1918=DIRECTION('',(0.,0.,-1.));
#1919=DIRECTION('',(1.,0.,0.));
#1920=DIRECTION('',(0.,0.,-1.));
#1921=DIRECTION('center_axis',(0.,1.,0.));
#1922=DIRECTION('ref_axis',(0.,0.,1.));
#1923=DIRECTION('',(1.,0.,0.));
#1924=DIRECTION('',(0.,0.,-1.));
#1925=DIRECTION('',(1.,0.,0.));
#1926=DIRECTION('',(0.,0.,-1.));
#1927=DIRECTION('center_axis',(0.,1.,0.));
#1928=DIRECTION('ref_axis',(0.,0.,1.));
#1929=DIRECTION('',(1.,0.,0.));
#1930=DIRECTION('',(0.,0.,-1.));
#1931=DIRECTION('',(-1.,0.,0.));
#1932=DIRECTION('',(0.,0.,-1.));
#1933=DIRECTION('',(-1.,0.,0.));
#1934=DIRECTION('',(0.,0.,1.));
#1935=DIRECTION('',(1.,0.,0.));
#1936=DIRECTION('',(0.,0.,-1.));
#1937=DIRECTION('center_axis',(0.,1.,0.));
#1938=DIRECTION('ref_axis',(0.,0.,1.));
#1939=DIRECTION('',(0.,0.,-1.));
#1940=DIRECTION('',(1.,0.,0.));
#1941=DIRECTION('',(0.,0.,-1.));
#1942=DIRECTION('',(1.,0.,0.));
#1943=DIRECTION('',(0.,0.,-1.));
#1944=DIRECTION('',(1.,0.,0.));
#1945=DIRECTION('',(0.,0.,1.));
#1946=DIRECTION('',(1.,0.,0.));
#1947=DIRECTION('center_axis',(0.,0.,-1.));
#1948=DIRECTION('ref_axis',(-1.,0.,0.));
#1949=DIRECTION('',(-1.,0.,0.));
#1950=DIRECTION('',(0.,1.,0.));
#1951=DIRECTION('',(0.,-1.,0.));
#1952=DIRECTION('',(0.,1.,0.));
#1953=DIRECTION('center_axis',(0.,0.,1.));
#1954=DIRECTION('ref_axis',(1.,0.,0.));
#1955=DIRECTION('',(-1.,0.,0.));
#1956=DIRECTION('',(0.,1.,0.));
#1957=DIRECTION('',(0.,-1.,0.));
#1958=DIRECTION('',(0.,-1.,0.));
#1959=DIRECTION('center_axis',(1.,0.,0.));
#1960=DIRECTION('ref_axis',(0.,0.,-1.));
#1961=DIRECTION('',(0.,1.,0.));
#1962=DIRECTION('',(0.,0.,-1.));
#1963=DIRECTION('',(0.,-1.,0.));
#1964=DIRECTION('',(0.,0.,1.));
#1965=DIRECTION('',(0.,1.,0.));
#1966=DIRECTION('center_axis',(-1.,0.,0.));
#1967=DIRECTION('ref_axis',(0.,0.,1.));
#1968=DIRECTION('',(0.,0.,1.));
#1969=DIRECTION('',(0.,1.,0.));
#1970=DIRECTION('',(0.,1.,0.));
#1971=DIRECTION('',(0.,0.,1.));
#1972=DIRECTION('',(0.,1.,0.));
#1973=DIRECTION('center_axis',(0.,0.,1.));
#1974=DIRECTION('ref_axis',(1.,0.,0.));
#1975=DIRECTION('',(-0.270221787772536,-0.962798102102935,0.));
#1976=DIRECTION('center_axis',(0.,0.,-1.));
#1977=DIRECTION('ref_axis',(1.,1.15648231731787E-14,0.));
#1978=DIRECTION('',(0.,1.,0.));
#1979=DIRECTION('center_axis',(0.,0.,-1.));
#1980=DIRECTION('ref_axis',(1.,5.72458747072346E-14,0.));
#1981=DIRECTION('center_axis',(0.,0.,1.));
#1982=DIRECTION('ref_axis',(1.,0.,0.));
#1983=DIRECTION('',(0.962798102102935,-0.270221787772537,0.));
#1984=DIRECTION('',(0.962798102102935,-0.270221787772537,0.));
#1985=DIRECTION('',(0.270221787772547,0.962798102102932,0.));
#1986=DIRECTION('center_axis',(0.,0.,-1.));
#1987=DIRECTION('ref_axis',(-1.,0.,0.));
#1988=DIRECTION('center_axis',(0.,0.,-1.));
#1989=DIRECTION('ref_axis',(1.,1.15648231731787E-14,0.));
#1990=DIRECTION('',(0.270221787772536,0.962798102102935,0.));
#1991=DIRECTION('center_axis',(0.,0.,-1.));
#1992=DIRECTION('ref_axis',(1.,5.72458747072346E-14,0.));
#1993=DIRECTION('center_axis',(0.,0.,1.));
#1994=DIRECTION('ref_axis',(1.,0.,0.));
#1995=DIRECTION('',(0.,-1.,0.));
#1996=DIRECTION('center_axis',(0.,0.,1.));
#1997=DIRECTION('ref_axis',(-1.,1.11022302462516E-13,0.));
#1998=DIRECTION('center_axis',(0.,0.,1.));
#1999=DIRECTION('ref_axis',(1.,0.,0.));
#2000=DIRECTION('center_axis',(0.,0.,1.));
#2001=DIRECTION('ref_axis',(1.,0.,0.));
#2002=DIRECTION('',(1.,0.,0.));
#2003=DIRECTION('',(1.,0.,0.));
#2004=DIRECTION('',(0.,1.,0.));
#2005=DIRECTION('center_axis',(0.,0.,-1.));
#2006=DIRECTION('ref_axis',(-1.,0.,0.));
#2007=DIRECTION('',(-0.270221787772547,-0.962798102102932,0.));
#2008=DIRECTION('center_axis',(0.,0.,1.));
#2009=DIRECTION('ref_axis',(-1.,1.11022302462516E-13,0.));
#2010=DIRECTION('',(0.,1.,0.));
#2011=DIRECTION('center_axis',(0.,0.,1.));
#2012=DIRECTION('ref_axis',(1.,0.,0.));
#2013=DIRECTION('center_axis',(0.,0.,-1.));
#2014=DIRECTION('ref_axis',(-1.,0.,0.));
#2015=DIRECTION('',(0.962798102102935,-0.270221787772537,0.));
#2016=DIRECTION('',(0.962798102102935,-0.270221787772537,0.));
#2017=DIRECTION('center_axis',(0.,0.,1.));
#2018=DIRECTION('ref_axis',(1.,0.,0.));
#2019=DIRECTION('',(0.27022178777254,-0.962798102102934,0.));
#2020=DIRECTION('center_axis',(0.,0.,1.));
#2021=DIRECTION('ref_axis',(-1.,2.08166817117217E-14,0.));
#2022=DIRECTION('center_axis',(0.,0.,1.));
#2023=DIRECTION('ref_axis',(1.,0.,0.));
#2024=DIRECTION('center_axis',(0.,0.,1.));
#2025=DIRECTION('ref_axis',(1.,0.,0.));
#2026=DIRECTION('',(0.962798102102935,0.270221787772537,0.));
#2027=DIRECTION('',(0.962798102102935,0.270221787772537,0.));
#2028=DIRECTION('',(-0.270221787772533,0.962798102102936,0.));
#2029=DIRECTION('center_axis',(0.,0.,-1.));
#2030=DIRECTION('ref_axis',(-1.,0.,0.));
#2031=DIRECTION('',(0.,-1.,0.));
#2032=DIRECTION('center_axis',(0.,0.,1.));
#2033=DIRECTION('ref_axis',(-1.,2.08166817117217E-14,0.));
#2034=DIRECTION('',(-0.27022178777254,0.962798102102934,0.));
#2035=DIRECTION('center_axis',(0.,0.,1.));
#2036=DIRECTION('ref_axis',(1.,0.,0.));
#2037=DIRECTION('center_axis',(0.,0.,-1.));
#2038=DIRECTION('ref_axis',(-1.,0.,0.));
#2039=DIRECTION('',(1.,0.,0.));
#2040=DIRECTION('',(1.,0.,0.));
#2041=DIRECTION('center_axis',(0.,0.,1.));
#2042=DIRECTION('ref_axis',(1.,0.,0.));
#2043=DIRECTION('center_axis',(0.,0.,-1.));
#2044=DIRECTION('ref_axis',(1.,4.48431918959993E-15,0.));
#2045=DIRECTION('center_axis',(0.,0.,-1.));
#2046=DIRECTION('ref_axis',(1.,-1.12757025938492E-14,0.));
#2047=DIRECTION('center_axis',(0.,0.,-1.));
#2048=DIRECTION('ref_axis',(-1.,0.,0.));
#2049=DIRECTION('',(0.270221787772533,-0.962798102102936,0.));
#2050=DIRECTION('center_axis',(0.,0.,-1.));
#2051=DIRECTION('ref_axis',(1.,4.48431918959993E-15,0.));
#2052=DIRECTION('',(0.,1.,0.));
#2053=DIRECTION('center_axis',(0.,0.,-1.));
#2054=DIRECTION('ref_axis',(1.,-1.12757025938492E-14,0.));
#2055=DIRECTION('center_axis',(0.,0.,-1.));
#2056=DIRECTION('ref_axis',(-1.,0.,0.));
#2057=DIRECTION('',(0.962798102102935,0.270221787772537,0.));
#2058=DIRECTION('',(0.962798102102935,0.270221787772537,0.));
#2059=DIRECTION('center_axis',(0.,0.,-1.));
#2060=DIRECTION('ref_axis',(-1.,0.,0.));
#2061=DIRECTION('',(0.,0.,-1.));
#2062=DIRECTION('center_axis',(-0.270221787772537,0.962798102102935,0.));
#2063=DIRECTION('ref_axis',(-0.962798102102935,-0.270221787772537,0.));
#2064=DIRECTION('',(0.,0.,-1.));
#2065=DIRECTION('center_axis',(0.,0.,-1.));
#2066=DIRECTION('ref_axis',(-1.,0.,0.));
#2067=DIRECTION('',(0.,0.,-1.));
#2068=DIRECTION('center_axis',(0.,1.,0.));
#2069=DIRECTION('ref_axis',(0.,0.,1.));
#2070=DIRECTION('',(0.,0.,-1.));
#2071=DIRECTION('center_axis',(0.,0.,-1.));
#2072=DIRECTION('ref_axis',(-1.,0.,0.));
#2073=DIRECTION('',(0.,0.,-1.));
#2074=DIRECTION('center_axis',(0.270221787772537,0.962798102102935,0.));
#2075=DIRECTION('ref_axis',(-0.962798102102935,0.270221787772537,0.));
#2076=DIRECTION('',(0.,0.,-1.));
#2077=DIRECTION('center_axis',(0.,0.,-1.));
#2078=DIRECTION('ref_axis',(-1.,0.,0.));
#2079=DIRECTION('center_axis',(0.,0.,-1.));
#2080=DIRECTION('ref_axis',(-1.,0.,0.));
#2081=DIRECTION('',(0.,0.,-1.));
#2082=DIRECTION('center_axis',(0.270221787772537,0.962798102102935,0.));
#2083=DIRECTION('ref_axis',(-0.962798102102935,0.270221787772537,0.));
#2084=DIRECTION('',(0.,0.,-1.));
#2085=DIRECTION('center_axis',(0.,0.,-1.));
#2086=DIRECTION('ref_axis',(-1.,0.,0.));
#2087=DIRECTION('',(0.,0.,-1.));
#2088=DIRECTION('center_axis',(0.,1.,0.));
#2089=DIRECTION('ref_axis',(0.,0.,1.));
#2090=DIRECTION('',(0.,0.,-1.));
#2091=DIRECTION('center_axis',(0.,0.,-1.));
#2092=DIRECTION('ref_axis',(-1.,0.,0.));
#2093=DIRECTION('',(0.,0.,-1.));
#2094=DIRECTION('center_axis',(-0.270221787772537,0.962798102102935,0.));
#2095=DIRECTION('ref_axis',(-0.962798102102935,-0.270221787772537,0.));
#2096=DIRECTION('',(0.,0.,-1.));
#2097=DIRECTION('center_axis',(0.,0.,-1.));
#2098=DIRECTION('ref_axis',(-1.,0.,0.));
#2099=DIRECTION('center_axis',(0.,0.,1.));
#2100=DIRECTION('ref_axis',(1.,0.,0.));
#2101=DIRECTION('',(0.,1.,0.));
#2102=DIRECTION('',(1.,0.,0.));
#2103=DIRECTION('center_axis',(0.,0.,1.));
#2104=DIRECTION('ref_axis',(1.,0.,0.));
#2105=DIRECTION('',(0.,1.,0.));
#2106=DIRECTION('',(-1.,0.,0.));
#2107=DIRECTION('center_axis',(0.,0.,-1.));
#2108=DIRECTION('ref_axis',(-1.,0.,0.));
#2109=DIRECTION('',(-1.,0.,0.));
#2110=DIRECTION('',(0.,1.,0.));
#2111=DIRECTION('center_axis',(-1.,0.,0.));
#2112=DIRECTION('ref_axis',(0.,0.,1.));
#2113=DIRECTION('',(0.,0.,1.));
#2114=DIRECTION('center_axis',(0.,1.,0.));
#2115=DIRECTION('ref_axis',(0.,0.,1.));
#2116=DIRECTION('center_axis',(0.,0.,1.));
#2117=DIRECTION('ref_axis',(1.,0.,0.));
#2118=DIRECTION('',(1.,0.,0.));
#2119=DIRECTION('',(0.,1.,0.));
#2120=DIRECTION('center_axis',(1.,0.,0.));
#2121=DIRECTION('ref_axis',(0.,0.,-1.));
#2122=DIRECTION('',(0.,0.,-1.));
#2123=DIRECTION('center_axis',(0.,1.,0.));
#2124=DIRECTION('ref_axis',(0.,0.,1.));
#2125=DIRECTION('center_axis',(-1.,0.,0.));
#2126=DIRECTION('ref_axis',(0.,0.,1.));
#2127=DIRECTION('',(0.,0.,1.));
#2128=DIRECTION('',(0.,1.,0.));
#2129=DIRECTION('center_axis',(0.,0.,1.));
#2130=DIRECTION('ref_axis',(1.,0.,0.));
#2131=DIRECTION('',(1.,0.,0.));
#2132=DIRECTION('center_axis',(0.,1.,0.));
#2133=DIRECTION('ref_axis',(0.,0.,1.));
#2134=DIRECTION('center_axis',(1.,0.,0.));
#2135=DIRECTION('ref_axis',(0.,0.,-1.));
#2136=DIRECTION('',(0.,0.,-1.));
#2137=DIRECTION('',(0.,1.,0.));
#2138=DIRECTION('center_axis',(0.,0.,-1.));
#2139=DIRECTION('ref_axis',(-1.,0.,0.));
#2140=DIRECTION('',(-1.,0.,0.));
#2141=DIRECTION('center_axis',(0.,1.,0.));
#2142=DIRECTION('ref_axis',(0.,0.,1.));
#2143=DIRECTION('axis',(0.,0.,1.));
#2144=DIRECTION('refdir',(1.,0.,0.));
#2145=DIRECTION('center_axis',(-1.,1.35175512935379E-29,1.36592399683213E-16));
#2146=DIRECTION('ref_axis',(1.36592399683213E-16,3.34927423218511E-46,1.));
#2147=DIRECTION('center_axis',(1.,-1.35175512935379E-29,-1.00041722951373E-16));
#2148=DIRECTION('ref_axis',(-1.00041722951373E-16,-8.29003070754679E-46,
-1.));
#2149=DIRECTION('',(-1.,1.35175512935379E-29,1.36592399683213E-16));
#2150=DIRECTION('center_axis',(-1.,1.35175512935379E-29,1.36592399683213E-16));
#2151=DIRECTION('ref_axis',(1.36592399683213E-16,3.34927423218511E-46,1.));
#2152=DIRECTION('center_axis',(-1.,1.35175512935379E-29,1.36592399683213E-16));
#2153=DIRECTION('ref_axis',(1.36592399683213E-16,3.34927423218511E-46,1.));
#2154=DIRECTION('center_axis',(1.,-1.35175512935379E-29,-1.00041722951373E-16));
#2155=DIRECTION('ref_axis',(-1.00041722951373E-16,-8.29003070754679E-46,
-1.));
#2156=DIRECTION('',(-1.,1.35175512935379E-29,1.36592399683213E-16));
#2157=DIRECTION('center_axis',(-1.,1.35175512935379E-29,1.36592399683213E-16));
#2158=DIRECTION('ref_axis',(1.36592399683213E-16,3.34927423218511E-46,1.));
#2159=DIRECTION('center_axis',(1.,-1.35175512935379E-29,-1.36592399683213E-16));
#2160=DIRECTION('ref_axis',(-1.36592399683213E-16,-2.26327091223021E-30,
-1.));
#2161=DIRECTION('',(1.36592399683213E-16,2.26327091223021E-30,1.));
#2162=DIRECTION('',(1.3517551293538E-29,-1.,-2.26327091223024E-30));
#2163=DIRECTION('',(1.36592399683213E-16,2.26327091223021E-30,1.));
#2164=DIRECTION('',(1.3517551293538E-29,-1.,-2.26327091223024E-30));
#2165=DIRECTION('center_axis',(-1.36592399683213E-16,-2.26327091223021E-30,
-1.));
#2166=DIRECTION('ref_axis',(-1.,1.35175512935379E-29,1.36592399683213E-16));
#2167=DIRECTION('',(1.,-1.35175512935379E-29,-1.36592399683213E-16));
#2168=DIRECTION('',(1.3517551293538E-29,-1.,-2.26327091223024E-30));
#2169=DIRECTION('',(1.,-1.35175512935379E-29,-1.36592399683213E-16));
#2170=DIRECTION('center_axis',(-1.,1.35175512935379E-29,4.55307998944045E-17));
#2171=DIRECTION('ref_axis',(4.55307998944045E-17,2.26327091223021E-30,1.));
#2172=DIRECTION('',(-4.55307998944045E-17,-2.26327091223021E-30,-1.));
#2173=DIRECTION('',(1.3517551293538E-29,-1.,-2.26327091223024E-30));
#2174=DIRECTION('',(-4.55307998944045E-17,-2.26327091223021E-30,-1.));
#2175=DIRECTION('center_axis',(1.57845630207171E-16,2.26327091223021E-30,
1.));
#2176=DIRECTION('ref_axis',(1.,-1.35175512935379E-29,-1.57845630207171E-16));
#2177=DIRECTION('',(-1.,1.35175512935379E-29,1.57845630207171E-16));
#2178=DIRECTION('',(1.3517551293538E-29,-1.,-2.26327091223024E-30));
#2179=DIRECTION('',(-1.,1.35175512935379E-29,1.57845630207171E-16));
#2180=DIRECTION('',(1.3517551293538E-29,-1.,-2.26327091223024E-30));
#2181=DIRECTION('center_axis',(-1.,1.35175512935379E-29,2.00083445902746E-16));
#2182=DIRECTION('ref_axis',(2.00083445902746E-16,2.26327091223021E-30,1.));
#2183=DIRECTION('',(-2.00083445902746E-16,-2.26327091223021E-30,-1.));
#2184=DIRECTION('',(1.3517551293538E-29,-1.,-2.26327091223024E-30));
#2185=DIRECTION('',(-2.00083445902746E-16,-2.26327091223021E-30,-1.));
#2186=DIRECTION('center_axis',(-1.57845630207171E-16,-2.26327091223021E-30,
-1.));
#2187=DIRECTION('ref_axis',(-1.,1.35175512935379E-29,1.57845630207171E-16));
#2188=DIRECTION('',(1.,-1.35175512935379E-29,-1.57845630207171E-16));
#2189=DIRECTION('',(1.3517551293538E-29,-1.,-2.26327091223024E-30));
#2190=DIRECTION('',(1.,-1.35175512935379E-29,-1.57845630207171E-16));
#2191=DIRECTION('center_axis',(1.,-1.35175512935379E-29,-1.00041722951373E-16));
#2192=DIRECTION('ref_axis',(-1.00041722951373E-16,-2.26327091223021E-30,
-1.));
#2193=DIRECTION('',(1.00041722951373E-16,2.26327091223021E-30,1.));
#2194=DIRECTION('',(1.00041722951373E-16,2.26327091223021E-30,1.));
#2195=DIRECTION('center_axis',(1.36592399683213E-16,2.26327091223021E-30,
1.));
#2196=DIRECTION('ref_axis',(1.,-1.35175512935379E-29,-1.36592399683213E-16));
#2197=DIRECTION('',(-1.,1.35175512935379E-29,1.36592399683213E-16));
#2198=DIRECTION('',(-1.,1.35175512935379E-29,1.36592399683213E-16));
#2199=DIRECTION('center_axis',(-1.3517551293538E-29,1.,-2.26327091223021E-30));
#2200=DIRECTION('ref_axis',(-1.72563323017094E-31,2.26327091223021E-30,
1.));
#2201=DIRECTION('center_axis',(-1.3517551293538E-29,1.,-2.26327091223021E-30));
#2202=DIRECTION('ref_axis',(-1.72563323017094E-31,2.26327091223021E-30,
1.));
#2203=DIRECTION('axis',(0.,0.,1.));
#2204=DIRECTION('refdir',(1.,0.,0.));
#2205=DIRECTION('center_axis',(0.,1.,0.));
#2206=DIRECTION('ref_axis',(0.,0.,1.));
#2207=DIRECTION('',(1.,0.,0.));
#2208=DIRECTION('',(0.,0.,-1.));
#2209=DIRECTION('',(1.,0.,0.));
#2210=DIRECTION('',(0.,0.,-1.));
#2211=DIRECTION('center_axis',(-1.,0.,0.));
#2212=DIRECTION('ref_axis',(0.,0.,1.));
#2213=DIRECTION('',(0.,1.,0.));
#2214=DIRECTION('',(0.,0.,-1.));
#2215=DIRECTION('',(0.,1.,0.));
#2216=DIRECTION('center_axis',(0.,-1.,0.));
#2217=DIRECTION('ref_axis',(0.,0.,-1.));
#2218=DIRECTION('',(-1.,0.,0.));
#2219=DIRECTION('',(0.,0.,-1.));
#2220=DIRECTION('',(-1.,0.,0.));
#2221=DIRECTION('center_axis',(0.266610574094054,-0.963804337913686,0.));
#2222=DIRECTION('ref_axis',(0.963804337913686,0.266610574094054,0.));
#2223=DIRECTION('',(-0.963804337913686,-0.266610574094054,0.));
#2224=DIRECTION('',(0.,0.,-1.));
#2225=DIRECTION('',(-0.963804337913686,-0.266610574094054,0.));
#2226=DIRECTION('center_axis',(0.,-1.,0.));
#2227=DIRECTION('ref_axis',(0.,0.,-1.));
#2228=DIRECTION('',(-1.,0.,0.));
#2229=DIRECTION('',(0.,0.,-1.));
#2230=DIRECTION('',(-1.,0.,0.));
#2231=DIRECTION('center_axis',(-0.26994323774403,-0.962876237320389,0.));
#2232=DIRECTION('ref_axis',(0.962876237320389,-0.26994323774403,0.));
#2233=DIRECTION('',(-0.962876237320389,0.26994323774403,0.));
#2234=DIRECTION('',(0.,0.,-1.));
#2235=DIRECTION('',(-0.962876237320389,0.26994323774403,0.));
#2236=DIRECTION('center_axis',(0.,-1.,0.));
#2237=DIRECTION('ref_axis',(0.,0.,-1.));
#2238=DIRECTION('',(-1.,0.,0.));
#2239=DIRECTION('',(0.,0.,-1.));
#2240=DIRECTION('',(-1.,0.,0.));
#2241=DIRECTION('center_axis',(1.,0.,0.));
#2242=DIRECTION('ref_axis',(0.,0.,-1.));
#2243=DIRECTION('',(0.,-1.,0.));
#2244=DIRECTION('',(0.,-1.,0.));
#2245=DIRECTION('center_axis',(0.,0.,-1.));
#2246=DIRECTION('ref_axis',(-1.,0.,0.));
#2247=DIRECTION('center_axis',(0.,0.,-1.));
#2248=DIRECTION('ref_axis',(-1.,0.,0.));
#2249=DIRECTION('axis',(0.,0.,1.));
#2250=DIRECTION('refdir',(1.,0.,0.));
#2251=DIRECTION('center_axis',(1.,-4.72726926582308E-31,-2.33146835171283E-15));
#2252=DIRECTION('ref_axis',(-2.33146835171283E-15,3.69778549322349E-30,
-1.));
#2253=DIRECTION('',(4.7272692658233E-31,-1.,3.54987407349459E-30));
#2254=DIRECTION('',(-2.33146835171283E-15,3.69778549322349E-30,-1.));
#2255=DIRECTION('',(4.7272692658233E-31,-1.,3.54987407349459E-30));
#2256=DIRECTION('',(-2.33146835171283E-15,3.69778549322349E-30,-1.));
#2257=DIRECTION('center_axis',(-4.72726926582313E-31,1.,3.69778549322349E-30));
#2258=DIRECTION('ref_axis',(2.33146835171283E-15,-3.69778549322349E-30,
1.));
#2259=DIRECTION('',(1.,-4.72726926582326E-31,2.33146835171283E-15));
#2260=DIRECTION('',(-2.33146835171283E-15,3.69778549322349E-30,-1.));
#2261=DIRECTION('',(1.,-4.72726926582326E-31,2.33146835171283E-15));
#2262=DIRECTION('center_axis',(-1.,4.72726926582308E-31,2.33146835171283E-15));
#2263=DIRECTION('ref_axis',(2.33146835171283E-15,-3.69778549322349E-30,
1.));
#2264=DIRECTION('',(-4.7272692658233E-31,1.,-3.54987407349459E-30));
#2265=DIRECTION('',(-2.33146835171283E-15,3.69778549322349E-30,-1.));
#2266=DIRECTION('',(-4.7272692658233E-31,1.,-3.54987407349459E-30));
#2267=DIRECTION('center_axis',(4.72726926582313E-31,-1.,-3.69778549322349E-30));
#2268=DIRECTION('ref_axis',(-2.33146835171283E-15,3.69778549322349E-30,
-1.));
#2269=DIRECTION('',(-1.,4.72726926582326E-31,-2.33146835171283E-15));
#2270=DIRECTION('',(-1.,4.72726926582326E-31,-2.33146835171283E-15));
#2271=DIRECTION('center_axis',(2.33146835171283E-15,3.69778549322349E-30,
-1.));
#2272=DIRECTION('ref_axis',(-1.,4.72726926582325E-31,-2.33146835171283E-15));
#2273=DIRECTION('center_axis',(2.33146835171283E-15,3.69778549322349E-30,
-1.));
#2274=DIRECTION('ref_axis',(-1.,4.72726926582325E-31,-2.33146835171283E-15));
#2275=DIRECTION('axis',(0.,0.,1.));
#2276=DIRECTION('refdir',(1.,0.,0.));
#2277=DIRECTION('center_axis',(6.34239344602916E-18,1.46822901856177E-15,
-1.));
#2278=DIRECTION('ref_axis',(-1.,-3.13984949151806E-15,-6.34239344603377E-18));
#2279=DIRECTION('center_axis',(6.34239344602916E-18,1.46822901856177E-15,
-1.));
#2280=DIRECTION('ref_axis',(1.,3.13984949151806E-15,6.34239344603377E-18));
#2281=DIRECTION('',(0.707106781186546,3.1718079570939E-15,-0.707106781186549));
#2282=DIRECTION('center_axis',(-6.34239344602916E-18,-1.46822901856177E-15,
1.));
#2283=DIRECTION('ref_axis',(1.,3.13984949151806E-15,6.34239344603377E-18));
#2284=DIRECTION('center_axis',(6.34239344602916E-18,1.46822901856177E-15,
-1.));
#2285=DIRECTION('ref_axis',(-1.,-3.13984949151806E-15,-6.34239344603377E-18));
#2286=DIRECTION('center_axis',(-6.34239344602916E-18,-1.46822901856177E-15,
1.));
#2287=DIRECTION('ref_axis',(1.,3.13984949151806E-15,6.34239344603377E-18));
#2288=DIRECTION('',(6.34239344602916E-18,1.46822901856177E-15,-1.));
#2289=DIRECTION('center_axis',(6.34239344602916E-18,1.46822901856177E-15,
-1.));
#2290=DIRECTION('ref_axis',(-1.,-3.13984949151806E-15,-6.34239344603377E-18));
#2291=DIRECTION('center_axis',(-6.34239344602916E-18,-1.46822901856177E-15,
1.));
#2292=DIRECTION('ref_axis',(1.,3.13984949151806E-15,6.34239344603377E-18));
#2293=DIRECTION('',(-6.34239344602916E-18,-1.46822901856177E-15,1.));
#2294=DIRECTION('center_axis',(-6.34239344602916E-18,-1.46822901856177E-15,
1.));
#2295=DIRECTION('ref_axis',(1.,3.13984949151806E-15,6.34239344603377E-18));
#2296=DIRECTION('center_axis',(6.34239344603457E-18,-1.46822901856177E-15,
1.));
#2297=DIRECTION('ref_axis',(1.,3.13984949151806E-15,-6.34239344602996E-18));
#2298=DIRECTION('center_axis',(6.34239344603457E-18,-1.46822901856177E-15,
1.));
#2299=DIRECTION('ref_axis',(1.,3.13984949151806E-15,-6.34239344602996E-18));
#2300=DIRECTION('',(0.,0.,1.));
#2301=DIRECTION('',(1.,0.,0.));
#2302=DIRECTION('',(-1.,1.66533453693773E-16,1.68639770869074E-32));
#2303=DIRECTION('',(-1.66533453693773E-16,-1.,2.46519032881566E-32));
#2304=DIRECTION('',(1.11022302462516E-16,-1.,2.14805035305496E-18));
#2305=DIRECTION('',(-0.0196550273413922,-3.45109949439587E-20,0.999806821291098));
#2306=DIRECTION('',(0.,0.,1.));
#2307=DIRECTION('',(1.,0.,0.));
#2308=DIRECTION('',(-2.20506388924687E-48,1.,-2.06061454873963E-16));
#2309=DIRECTION('',(1.,1.08712516854687E-48,-5.42526850246586E-33));
#2310=DIRECTION('',(-1.,1.11022302462516E-16,3.33561035819506E-48));
#2311=DIRECTION('',(-1.11022302462516E-16,-1.,-2.46519032881566E-32));
#2312=DIRECTION('',(0.,0.,1.));
#2313=DIRECTION('',(1.,0.,0.));
#2314=DIRECTION('',(-2.20506388924687E-48,1.,-2.06061454873963E-16));
#2315=DIRECTION('',(1.,1.08712516854687E-48,-5.42526850246586E-33));
#2316=DIRECTION('',(-2.20506388924687E-48,1.,-2.06061454873963E-16));
#2317=DIRECTION('',(1.,1.08712516854687E-48,-5.42526850246586E-33));
#2318=DIRECTION('',(5.55111512312578E-17,1.,-2.06061454873963E-16));
#2319=DIRECTION('',(1.,-5.55111512312578E-17,-5.47382212626882E-48));
#2320=DIRECTION('',(5.55111512312578E-17,1.,-2.06061454873963E-16));
#2321=DIRECTION('',(1.,-5.55111512312578E-17,-5.47382212626882E-48));
#2322=DIRECTION('',(5.55111512312578E-17,1.,-2.06061454873963E-16));
#2323=DIRECTION('',(1.,-5.55111512312578E-17,-5.47382212626882E-48));
#2324=DIRECTION('',(1.11022302462516E-16,-1.,2.14805035305496E-18));
#2325=DIRECTION('',(-0.0196550273413922,-3.45109949439587E-20,0.999806821291098));
#2326=DIRECTION('',(1.11022302462516E-16,-1.,2.14805035305496E-18));
#2327=DIRECTION('',(-0.0196550273413922,-3.45109949439587E-20,0.999806821291098));
#2328=DIRECTION('',(1.11022302462516E-16,-1.,2.14805035305496E-18));
#2329=DIRECTION('',(-0.0196550273413922,-3.45109949439587E-20,0.999806821291098));
#2330=CARTESIAN_POINT('',(0.,0.,0.));
#2331=CARTESIAN_POINT('',(0.,0.,0.));
#2332=CARTESIAN_POINT('Origin',(575.,7.00000000000001,12.7000000000002));
#2333=CARTESIAN_POINT('',(575.,-3.,19.7000000000001));
#2334=CARTESIAN_POINT('Origin',(575.,-3.,12.7000000000002));
#2335=CARTESIAN_POINT('',(575.,-6.34999999999999,19.7000000000001));
#2336=CARTESIAN_POINT('',(575.,7.00000000000001,19.7000000000001));
#2337=CARTESIAN_POINT('Origin',(575.,-6.34999999999999,12.7000000000002));
#2338=CARTESIAN_POINT('Origin',(25.,7.00000000000001,974.6));
#2339=CARTESIAN_POINT('',(25.,-3.,981.6));
#2340=CARTESIAN_POINT('Origin',(25.,-3.,974.6));
#2341=CARTESIAN_POINT('',(25.,-6.34999999999999,981.6));
#2342=CARTESIAN_POINT('',(25.,7.00000000000001,981.6));
#2343=CARTESIAN_POINT('Origin',(25.,-6.34999999999999,974.6));
#2344=CARTESIAN_POINT('Origin',(25.,7.00000000000001,12.7000000000002));
#2345=CARTESIAN_POINT('',(25.,-3.,19.7000000000001));
#2346=CARTESIAN_POINT('Origin',(25.,-3.,12.7000000000002));
#2347=CARTESIAN_POINT('',(25.,-6.34999999999999,19.7000000000001));
#2348=CARTESIAN_POINT('',(25.,7.00000000000001,19.7000000000001));
#2349=CARTESIAN_POINT('Origin',(25.,-6.34999999999999,12.7000000000002));
#2350=CARTESIAN_POINT('Origin',(575.,7.00000000000001,974.6));
#2351=CARTESIAN_POINT('',(575.,-3.,981.6));
#2352=CARTESIAN_POINT('Origin',(575.,-3.,974.6));
#2353=CARTESIAN_POINT('',(575.,-6.34999999999999,981.6));
#2354=CARTESIAN_POINT('',(575.,7.00000000000001,981.6));
#2355=CARTESIAN_POINT('Origin',(575.,-6.34999999999999,974.6));
#2356=CARTESIAN_POINT('Origin',(562.5,-10.,50.));
#2357=CARTESIAN_POINT('',(562.5,-6.34999999999999,28.5));
#2358=CARTESIAN_POINT('Origin',(562.5,-6.34999999999999,50.));
#2359=CARTESIAN_POINT('',(562.5,0.,28.5));
#2360=CARTESIAN_POINT('',(562.5,-10.,28.5));
#2361=CARTESIAN_POINT('Origin',(562.5,0.,50.));
#2362=CARTESIAN_POINT('Origin',(562.5,-10.,937.3));
#2363=CARTESIAN_POINT('',(562.5,-6.34999999999999,915.8));
#2364=CARTESIAN_POINT('Origin',(562.5,-6.34999999999999,937.3));
#2365=CARTESIAN_POINT('',(562.5,0.,915.8));
#2366=CARTESIAN_POINT('',(562.5,-10.,915.8));
#2367=CARTESIAN_POINT('Origin',(562.5,0.,937.3));
#2368=CARTESIAN_POINT('Origin',(37.4999999999998,-10.,937.3));
#2369=CARTESIAN_POINT('',(37.4999999999998,-6.34999999999999,915.8));
#2370=CARTESIAN_POINT('Origin',(37.4999999999998,-6.34999999999999,937.3));
#2371=CARTESIAN_POINT('',(37.4999999999998,0.,915.8));
#2372=CARTESIAN_POINT('',(37.4999999999998,-10.,915.8));
#2373=CARTESIAN_POINT('Origin',(37.4999999999998,0.,937.3));
#2374=CARTESIAN_POINT('Origin',(37.4999999999998,-10.,50.));
#2375=CARTESIAN_POINT('',(37.4999999999998,-6.34999999999999,28.5));
#2376=CARTESIAN_POINT('Origin',(37.4999999999998,-6.34999999999999,50.));
#2377=CARTESIAN_POINT('',(37.4999999999998,0.,28.5));
#2378=CARTESIAN_POINT('',(37.4999999999998,-10.,28.5));
#2379=CARTESIAN_POINT('Origin',(37.4999999999998,0.,50.));
#2380=CARTESIAN_POINT('Origin',(520.,-6.34999999999999,987.3));
#2381=CARTESIAN_POINT('',(521.011887130928,-6.34999999999999,0.));
#2382=CARTESIAN_POINT('',(600.,-6.34999999999999,0.));
#2383=CARTESIAN_POINT('',(520.,-6.34999999999999,0.));
#2384=CARTESIAN_POINT('',(600.,-6.34999999999999,987.3));
#2385=CARTESIAN_POINT('',(600.,-6.34999999999999,987.3));
#2386=CARTESIAN_POINT('',(521.011887130928,-6.34999999999999,987.3));
#2387=CARTESIAN_POINT('',(520.,-6.34999999999999,987.3));
#2388=CARTESIAN_POINT('',(521.011887130928,-6.34999999999999,987.3));
#2389=CARTESIAN_POINT('Origin',(0.,-6.34999999999999,987.3));
#2390=CARTESIAN_POINT('',(0.,-6.34999999999999,0.));
#2391=CARTESIAN_POINT('',(78.9881128690719,-6.34999999999999,0.));
#2392=CARTESIAN_POINT('',(0.,-6.34999999999999,0.));
#2393=CARTESIAN_POINT('',(78.9881128690719,-6.34999999999999,987.3));
#2394=CARTESIAN_POINT('',(78.9881128690719,-6.34999999999999,987.3));
#2395=CARTESIAN_POINT('',(0.,-6.34999999999999,987.3));
#2396=CARTESIAN_POINT('',(0.,-6.34999999999999,987.3));
#2397=CARTESIAN_POINT('',(0.,-6.34999999999999,987.3));
#2398=CARTESIAN_POINT('Origin',(520.,0.,987.3));
#2399=CARTESIAN_POINT('',(521.011887130928,0.,987.3));
#2400=CARTESIAN_POINT('',(555.,0.,987.3));
#2401=CARTESIAN_POINT('',(520.,0.,987.3));
#2402=CARTESIAN_POINT('',(555.,0.,962.3));
#2403=CARTESIAN_POINT('',(555.,0.,0.));
#2404=CARTESIAN_POINT('',(600.,0.,962.3));
#2405=CARTESIAN_POINT('',(0.,0.,962.3));
#2406=CARTESIAN_POINT('',(600.,0.,25.));
#2407=CARTESIAN_POINT('',(600.,0.,987.3));
#2408=CARTESIAN_POINT('',(555.,0.,25.));
#2409=CARTESIAN_POINT('',(0.,0.,25.));
#2410=CARTESIAN_POINT('',(555.,0.,0.));
#2411=CARTESIAN_POINT('',(555.,0.,0.));
#2412=CARTESIAN_POINT('',(521.011887130928,0.,0.));
#2413=CARTESIAN_POINT('',(520.,0.,0.));
#2414=CARTESIAN_POINT('',(521.011887130928,0.,987.3));
#2415=CARTESIAN_POINT('Origin',(0.,0.,987.3));
#2416=CARTESIAN_POINT('',(0.,0.,962.3));
#2417=CARTESIAN_POINT('',(0.,0.,25.));
#2418=CARTESIAN_POINT('',(0.,0.,987.3));
#2419=CARTESIAN_POINT('',(45.,0.,962.3));
#2420=CARTESIAN_POINT('',(0.,0.,962.3));
#2421=CARTESIAN_POINT('',(45.,0.,987.3));
#2422=CARTESIAN_POINT('',(45.,0.,0.));
#2423=CARTESIAN_POINT('',(78.9881128690719,0.,987.3));
#2424=CARTESIAN_POINT('',(0.,0.,987.3));
#2425=CARTESIAN_POINT('',(78.9881128690719,0.,0.));
#2426=CARTESIAN_POINT('',(78.9881128690719,0.,987.3));
#2427=CARTESIAN_POINT('',(44.9999999999999,0.,0.));
#2428=CARTESIAN_POINT('',(0.,0.,0.));
#2429=CARTESIAN_POINT('',(44.9999999999999,0.,25.));
#2430=CARTESIAN_POINT('',(44.9999999999999,0.,0.));
#2431=CARTESIAN_POINT('',(0.,0.,25.));
#2432=CARTESIAN_POINT('Origin',(79.2583346568445,-6.38720189789707,0.));
#2433=CARTESIAN_POINT('',(44.9999999999999,-3.,0.));
#2434=CARTESIAN_POINT('',(0.,-3.,0.));
#2435=CARTESIAN_POINT('',(0.,-3.,0.));
#2436=CARTESIAN_POINT('',(44.9999999999999,-3.,0.));
#2437=CARTESIAN_POINT('',(78.9881128690719,0.,0.));
#2438=CARTESIAN_POINT('',(0.,-6.34999999999999,0.));
#2439=CARTESIAN_POINT('Origin',(520.741665343155,-6.3872018978971,987.3));
#2440=CARTESIAN_POINT('',(600.,-3.,987.3));
#2441=CARTESIAN_POINT('',(555.,-3.,987.3));
#2442=CARTESIAN_POINT('',(0.,-3.,987.3));
#2443=CARTESIAN_POINT('',(555.,-3.,987.3));
#2444=CARTESIAN_POINT('',(521.011887130928,0.,987.3));
#2445=CARTESIAN_POINT('',(600.,0.,987.3));
#2446=CARTESIAN_POINT('Origin',(600.,0.,987.3));
#2447=CARTESIAN_POINT('',(600.,-3.,962.3));
#2448=CARTESIAN_POINT('',(600.,-3.,962.3));
#2449=CARTESIAN_POINT('',(600.,-3.,0.));
#2450=CARTESIAN_POINT('',(600.,-3.,0.));
#2451=CARTESIAN_POINT('',(600.,0.,0.));
#2452=CARTESIAN_POINT('',(600.,-3.,25.));
#2453=CARTESIAN_POINT('',(600.,-3.,0.));
#2454=CARTESIAN_POINT('',(600.,-3.,25.));
#2455=CARTESIAN_POINT('Origin',(0.,-6.34999999999999,987.3));
#2456=CARTESIAN_POINT('',(0.,-3.,962.3));
#2457=CARTESIAN_POINT('',(0.,-3.,987.3));
#2458=CARTESIAN_POINT('',(0.,-3.,0.));
#2459=CARTESIAN_POINT('',(0.,-3.,962.3));
#2460=CARTESIAN_POINT('',(0.,-3.,25.));
#2461=CARTESIAN_POINT('',(0.,-3.,25.));
#2462=CARTESIAN_POINT('',(0.,-3.,0.));
#2463=CARTESIAN_POINT('',(0.,-6.34999999999999,987.3));
#2464=CARTESIAN_POINT('Origin',(80.9742430092,-0.273433949543433,987.3));
#2465=CARTESIAN_POINT('',(80.9742430092,-0.273433949543433,987.3));
#2466=CARTESIAN_POINT('',(79.2583346568445,-6.38720189789707,987.3));
#2467=CARTESIAN_POINT('',(80.9742430092,-0.273433949543433,987.3));
#2468=CARTESIAN_POINT('Origin',(78.9881128690719,-7.35,987.3));
#2469=CARTESIAN_POINT('',(78.9881128690719,-6.34999999999999,987.3));
#2470=CARTESIAN_POINT('Origin',(78.9881128690719,-7.35,987.3));
#2471=CARTESIAN_POINT('Origin',(78.9881128690719,-6.34999999999999,987.3));
#2472=CARTESIAN_POINT('',(260.867449930721,-50.7627981021028,987.3));
#2473=CARTESIAN_POINT('',(80.,0.,987.3));
#2474=CARTESIAN_POINT('',(259.151541578365,-56.8765660504565,987.3));
#2475=CARTESIAN_POINT('',(78.2840916476444,-6.11376794835364,987.3));
#2476=CARTESIAN_POINT('',(259.151541578365,-56.8765660504565,987.3));
#2477=CARTESIAN_POINT('Origin',(78.9881128690719,0.,0.));
#2478=CARTESIAN_POINT('',(80.9742430092,-0.273433949543433,0.));
#2479=CARTESIAN_POINT('Origin',(78.9881128690719,-7.35,0.));
#2480=CARTESIAN_POINT('',(79.2583346568445,-6.38720189789707,0.));
#2481=CARTESIAN_POINT('',(79.2583346568445,-6.38720189789707,0.));
#2482=CARTESIAN_POINT('Origin',(78.9881128690719,-7.35,0.));
#2483=CARTESIAN_POINT('Origin',(261.137671718493,-50.8,987.3));
#2484=CARTESIAN_POINT('',(261.137671718493,-50.8,987.3));
#2485=CARTESIAN_POINT('',(261.137671718493,-57.15,987.3));
#2486=CARTESIAN_POINT('',(261.137671718493,-50.8,987.3));
#2487=CARTESIAN_POINT('Origin',(261.137671718493,-49.8,987.3));
#2488=CARTESIAN_POINT('Origin',(261.137671718493,-49.8,987.3));
#2489=CARTESIAN_POINT('Origin',(259.151541578365,-56.8765660504565,987.3));
#2490=CARTESIAN_POINT('',(338.862328281506,-50.8,987.3));
#2491=CARTESIAN_POINT('',(261.,-50.8,987.3));
#2492=CARTESIAN_POINT('',(338.862328281506,-57.15,987.3));
#2493=CARTESIAN_POINT('',(261.,-57.15,987.3));
#2494=CARTESIAN_POINT('',(338.862328281506,-57.15,987.3));
#2495=CARTESIAN_POINT('Origin',(260.867449930721,-50.7627981021028,0.));
#2496=CARTESIAN_POINT('',(260.867449930721,-50.7627981021028,0.));
#2497=CARTESIAN_POINT('',(259.151541578365,-56.8765660504565,0.));
#2498=CARTESIAN_POINT('',(260.867449930721,-50.7627981021028,0.));
#2499=CARTESIAN_POINT('',(261.137671718493,-50.8,0.));
#2500=CARTESIAN_POINT('Origin',(261.137671718493,-49.8,0.));
#2501=CARTESIAN_POINT('',(261.137671718493,-57.15,0.));
#2502=CARTESIAN_POINT('',(261.137671718493,-57.15,0.));
#2503=CARTESIAN_POINT('Origin',(261.137671718493,-49.8,0.));
#2504=CARTESIAN_POINT('Origin',(261.137671718493,-57.15,0.));
#2505=CARTESIAN_POINT('',(80.,0.,0.));
#2506=CARTESIAN_POINT('',(78.2840916476444,-6.11376794835364,0.));
#2507=CARTESIAN_POINT('Origin',(339.132550069279,-50.7627981021029,987.3));
#2508=CARTESIAN_POINT('',(339.132550069279,-50.7627981021029,987.3));
#2509=CARTESIAN_POINT('',(340.848458421635,-56.8765660504566,987.3));
#2510=CARTESIAN_POINT('',(339.132550069279,-50.7627981021029,987.3));
#2511=CARTESIAN_POINT('Origin',(338.862328281506,-49.8,987.3));
#2512=CARTESIAN_POINT('Origin',(338.862328281506,-49.8,987.3));
#2513=CARTESIAN_POINT('Origin',(338.862328281506,-57.15,987.3));
#2514=CARTESIAN_POINT('',(519.0257569908,-0.273433949543461,987.3));
#2515=CARTESIAN_POINT('',(339.,-50.8,987.3));
#2516=CARTESIAN_POINT('',(520.741665343155,-6.3872018978971,987.3));
#2517=CARTESIAN_POINT('',(340.715908352356,-56.9137679483536,987.3));
#2518=CARTESIAN_POINT('',(520.741665343155,-6.3872018978971,987.3));
#2519=CARTESIAN_POINT('Origin',(338.862328281506,-50.8,0.));
#2520=CARTESIAN_POINT('',(338.862328281506,-50.8,0.));
#2521=CARTESIAN_POINT('',(338.862328281506,-57.15,0.));
#2522=CARTESIAN_POINT('',(338.862328281506,-50.8,0.));
#2523=CARTESIAN_POINT('',(339.132550069279,-50.7627981021029,0.));
#2524=CARTESIAN_POINT('Origin',(338.862328281506,-49.8,0.));
#2525=CARTESIAN_POINT('',(340.848458421635,-56.8765660504566,0.));
#2526=CARTESIAN_POINT('',(340.848458421635,-56.8765660504566,0.));
#2527=CARTESIAN_POINT('Origin',(338.862328281506,-49.8,0.));
#2528=CARTESIAN_POINT('Origin',(340.848458421635,-56.8765660504566,0.));
#2529=CARTESIAN_POINT('',(261.,-50.8,0.));
#2530=CARTESIAN_POINT('',(261.,-57.15,0.));
#2531=CARTESIAN_POINT('Origin',(521.011887130928,0.,987.3));
#2532=CARTESIAN_POINT('Origin',(521.011887130928,-7.35000000000002,987.3));
#2533=CARTESIAN_POINT('Origin',(521.011887130928,-7.35000000000002,987.3));
#2534=CARTESIAN_POINT('Origin',(519.0257569908,-0.273433949543461,0.));
#2535=CARTESIAN_POINT('',(519.0257569908,-0.273433949543461,0.));
#2536=CARTESIAN_POINT('',(520.741665343155,-6.3872018978971,0.));
#2537=CARTESIAN_POINT('',(519.0257569908,-0.273433949543461,0.));
#2538=CARTESIAN_POINT('Origin',(521.011887130928,-7.35000000000002,0.));
#2539=CARTESIAN_POINT('',(521.011887130928,-6.34999999999999,0.));
#2540=CARTESIAN_POINT('Origin',(521.011887130928,-7.35000000000002,0.));
#2541=CARTESIAN_POINT('Origin',(521.011887130928,-6.34999999999999,0.));
#2542=CARTESIAN_POINT('',(339.,-50.8,0.));
#2543=CARTESIAN_POINT('',(340.715908352356,-56.9137679483536,0.));
#2544=CARTESIAN_POINT('Origin',(521.011887130928,-7.35000000000002,987.3));
#2545=CARTESIAN_POINT('',(519.0257569908,-0.273433949543461,987.3));
#2546=CARTESIAN_POINT('Origin',(339.,-50.8,987.3));
#2547=CARTESIAN_POINT('',(339.132550069279,-50.7627981021029,987.3));
#2548=CARTESIAN_POINT('Origin',(338.862328281506,-49.8,987.3));
#2549=CARTESIAN_POINT('',(338.862328281506,-50.8,987.3));
#2550=CARTESIAN_POINT('Origin',(261.,-50.8,987.3));
#2551=CARTESIAN_POINT('',(261.137671718493,-50.8,987.3));
#2552=CARTESIAN_POINT('Origin',(261.137671718493,-49.8,987.3));
#2553=CARTESIAN_POINT('',(260.867449930721,-50.7627981021028,987.3));
#2554=CARTESIAN_POINT('Origin',(80.,0.,987.3));
#2555=CARTESIAN_POINT('',(80.9742430092,-0.273433949543433,987.3));
#2556=CARTESIAN_POINT('Origin',(78.9881128690719,-7.35,987.3));
#2557=CARTESIAN_POINT('Origin',(78.9881128690719,-7.35,987.3));
#2558=CARTESIAN_POINT('',(79.2583346568445,-6.38720189789707,987.3));
#2559=CARTESIAN_POINT('Origin',(78.2840916476444,-6.11376794835364,987.3));
#2560=CARTESIAN_POINT('',(259.151541578365,-56.8765660504565,987.3));
#2561=CARTESIAN_POINT('Origin',(261.137671718493,-49.8,987.3));
#2562=CARTESIAN_POINT('',(261.137671718493,-57.15,987.3));
#2563=CARTESIAN_POINT('Origin',(261.,-57.15,987.3));
#2564=CARTESIAN_POINT('',(338.862328281506,-57.15,987.3));
#2565=CARTESIAN_POINT('Origin',(338.862328281506,-49.8,987.3));
#2566=CARTESIAN_POINT('',(340.848458421635,-56.8765660504566,987.3));
#2567=CARTESIAN_POINT('Origin',(340.715908352356,-56.9137679483536,987.3));
#2568=CARTESIAN_POINT('',(520.741665343155,-6.3872018978971,987.3));
#2569=CARTESIAN_POINT('Origin',(521.011887130928,-7.35000000000002,987.3));
#2570=CARTESIAN_POINT('Origin',(521.011887130928,-7.35000000000002,987.3));
#2571=CARTESIAN_POINT('',(45.,-3.,987.3));
#2572=CARTESIAN_POINT('',(45.,-3.,987.3));
#2573=CARTESIAN_POINT('',(0.,-3.,987.3));
#2574=CARTESIAN_POINT('Origin',(521.011887130928,-7.35000000000002,0.));
#2575=CARTESIAN_POINT('',(555.,-3.,0.));
#2576=CARTESIAN_POINT('',(555.,-3.,0.));
#2577=CARTESIAN_POINT('',(0.,-3.,0.));
#2578=CARTESIAN_POINT('Origin',(0.,-3.,25.));
#2579=CARTESIAN_POINT('',(555.,-3.,25.));
#2580=CARTESIAN_POINT('',(0.,-3.,25.));
#2581=CARTESIAN_POINT('',(555.,-3.,25.));
#2582=CARTESIAN_POINT('Origin',(555.,-3.,0.));
#2583=CARTESIAN_POINT('',(555.,-3.,0.));
#2584=CARTESIAN_POINT('Origin',(0.,-3.,0.));
#2585=CARTESIAN_POINT('Origin',(0.,-3.,962.3));
#2586=CARTESIAN_POINT('',(45.,-3.,962.3));
#2587=CARTESIAN_POINT('',(0.,-3.,962.3));
#2588=CARTESIAN_POINT('',(45.,-3.,962.3));
#2589=CARTESIAN_POINT('Origin',(45.,-3.,0.));
#2590=CARTESIAN_POINT('',(45.,-3.,0.));
#2591=CARTESIAN_POINT('Origin',(0.,-3.,0.));
#2592=CARTESIAN_POINT('Origin',(44.9999999999999,-3.,0.));
#2593=CARTESIAN_POINT('',(44.9999999999999,-3.,25.));
#2594=CARTESIAN_POINT('',(44.9999999999999,-3.,0.));
#2595=CARTESIAN_POINT('',(44.9999999999999,-3.,25.));
#2596=CARTESIAN_POINT('Origin',(0.,-3.,25.));
#2597=CARTESIAN_POINT('',(0.,-3.,25.));
#2598=CARTESIAN_POINT('Origin',(0.,-3.,0.));
#2599=CARTESIAN_POINT('Origin',(555.,-3.,0.));
#2600=CARTESIAN_POINT('',(555.,-3.,962.3));
#2601=CARTESIAN_POINT('',(555.,-3.,0.));
#2602=CARTESIAN_POINT('',(555.,-3.,962.3));
#2603=CARTESIAN_POINT('Origin',(0.,-3.,962.3));
#2604=CARTESIAN_POINT('',(0.,-3.,962.3));
#2605=CARTESIAN_POINT('Origin',(0.,-3.,0.));
#2606=CARTESIAN_POINT('',(0.,0.,0.));
#2607=CARTESIAN_POINT('Origin',(-15.4000000000002,937.3,0.600000000000211));
#2608=CARTESIAN_POINT('',(-21.9800000000002,937.3,-20.9));
#2609=CARTESIAN_POINT('Origin',(-21.9800000000002,937.3,0.600000000000211));
#2610=CARTESIAN_POINT('',(-25.4000000000003,937.3,-20.9));
#2611=CARTESIAN_POINT('',(-15.4000000000002,937.3,-20.9));
#2612=CARTESIAN_POINT('Origin',(-25.4000000000003,937.3,0.600000000000211));
#2613=CARTESIAN_POINT('Origin',(-15.4000000000002,50.,-0.6000000000001));
#2614=CARTESIAN_POINT('',(-21.9800000000002,50.,-22.1000000000003));
#2615=CARTESIAN_POINT('Origin',(-21.9800000000002,50.,-0.6000000000001));
#2616=CARTESIAN_POINT('',(-25.4000000000003,50.,-22.1000000000003));
#2617=CARTESIAN_POINT('',(-15.4000000000002,50.,-22.1000000000003));
#2618=CARTESIAN_POINT('Origin',(-25.4000000000003,50.,-0.6000000000001));
#2619=CARTESIAN_POINT('Origin',(-25.4000000000003,987.3,38.1000000000007));
#2620=CARTESIAN_POINT('',(-25.4000000000003,0.,-38.1000000000009));
#2621=CARTESIAN_POINT('',(-25.4000000000003,0.,38.1000000000007));
#2622=CARTESIAN_POINT('',(-25.4000000000003,0.,38.1000000000007));
#2623=CARTESIAN_POINT('',(-25.4000000000003,987.3,38.1000000000007));
#2624=CARTESIAN_POINT('',(-25.4000000000003,987.3,38.1000000000007));
#2625=CARTESIAN_POINT('',(-25.4000000000003,987.3,-38.1000000000009));
#2626=CARTESIAN_POINT('',(-25.4000000000003,987.3,38.1000000000007));
#2627=CARTESIAN_POINT('',(-25.4000000000003,987.3,-38.1000000000009));
#2628=CARTESIAN_POINT('Origin',(-25.4000000000003,987.3,38.1000000000007));
#2629=CARTESIAN_POINT('',(25.4000000000006,0.,38.1000000000014));
#2630=CARTESIAN_POINT('',(-25.4000000000003,0.,38.1000000000007));
#2631=CARTESIAN_POINT('',(25.4000000000006,987.3,38.1000000000014));
#2632=CARTESIAN_POINT('',(25.4000000000006,987.3,38.1000000000014));
#2633=CARTESIAN_POINT('',(-25.4000000000003,987.3,38.1000000000007));
#2634=CARTESIAN_POINT('Origin',(25.4000000000006,987.3,-38.1000000000007));
#2635=CARTESIAN_POINT('',(25.4000000000006,0.,-38.1000000000007));
#2636=CARTESIAN_POINT('',(25.4000000000006,0.,-38.1000000000007));
#2637=CARTESIAN_POINT('',(25.4000000000006,987.3,-38.1000000000007));
#2638=CARTESIAN_POINT('',(25.4000000000006,987.3,-38.1000000000007));
#2639=CARTESIAN_POINT('',(25.4000000000006,987.3,-38.1000000000007));
#2640=CARTESIAN_POINT('Origin',(21.9800000000002,987.3,-34.6800000000007));
#2641=CARTESIAN_POINT('',(21.9800000000002,0.,-34.6800000000007));
#2642=CARTESIAN_POINT('',(-21.9800000000002,0.,-34.6800000000009));
#2643=CARTESIAN_POINT('',(21.9800000000002,0.,-34.6800000000007));
#2644=CARTESIAN_POINT('',(21.9800000000002,987.3,-34.6800000000007));
#2645=CARTESIAN_POINT('',(21.9800000000002,987.3,-34.6800000000007));
#2646=CARTESIAN_POINT('',(-21.9800000000002,987.3,-34.6800000000009));
#2647=CARTESIAN_POINT('',(21.9800000000002,987.3,-34.6800000000007));
#2648=CARTESIAN_POINT('',(-21.9800000000002,987.3,-34.6800000000009));
#2649=CARTESIAN_POINT('Origin',(21.9800000000002,987.3,-34.6800000000007));
#2650=CARTESIAN_POINT('',(21.9800000000003,0.,34.6800000000014));
#2651=CARTESIAN_POINT('',(21.9800000000002,0.,-34.6800000000007));
#2652=CARTESIAN_POINT('',(21.9800000000003,987.3,34.6800000000014));
#2653=CARTESIAN_POINT('',(21.9800000000003,987.3,34.6800000000014));
#2654=CARTESIAN_POINT('',(21.9800000000002,987.3,-34.6800000000007));
#2655=CARTESIAN_POINT('Origin',(-21.9800000000001,987.3,34.6800000000008));
#2656=CARTESIAN_POINT('',(-21.9800000000001,0.,34.6800000000008));
#2657=CARTESIAN_POINT('',(-21.9800000000001,0.,34.6800000000008));
#2658=CARTESIAN_POINT('',(-21.9800000000001,987.3,34.6800000000008));
#2659=CARTESIAN_POINT('',(-21.9800000000001,987.3,34.6800000000008));
#2660=CARTESIAN_POINT('',(-21.9800000000001,987.3,34.6800000000008));
#2661=CARTESIAN_POINT('Origin',(-21.9800000000001,987.3,34.6800000000008));
#2662=CARTESIAN_POINT('',(-21.9800000000001,0.,34.6800000000008));
#2663=CARTESIAN_POINT('',(-21.9800000000001,987.3,34.6800000000008));
#2664=CARTESIAN_POINT('Origin',(25.4000000000006,987.3,-38.1000000000007));
#2665=CARTESIAN_POINT('',(25.4000000000006,0.,-38.1000000000007));
#2666=CARTESIAN_POINT('',(25.4000000000006,987.3,-38.1000000000007));
#2667=CARTESIAN_POINT('Origin',(0.,987.3,0.));
#2668=CARTESIAN_POINT('Origin',(0.,0.,0.));
#2669=CARTESIAN_POINT('',(0.,0.,0.));
#2670=CARTESIAN_POINT('Origin',(600.,0.,6.35000000000008));
#2671=CARTESIAN_POINT('',(0.,0.,0.));
#2672=CARTESIAN_POINT('',(600.,0.,0.));
#2673=CARTESIAN_POINT('',(600.,0.,0.));
#2674=CARTESIAN_POINT('',(600.,0.,6.35000000000008));
#2675=CARTESIAN_POINT('',(600.,0.,6.35000000000008));
#2676=CARTESIAN_POINT('',(0.,0.,6.35000000000008));
#2677=CARTESIAN_POINT('',(600.,0.,6.35000000000008));
#2678=CARTESIAN_POINT('',(0.,0.,6.35000000000008));
#2679=CARTESIAN_POINT('Origin',(600.,57.0813206381415,6.35000000000008));
#2680=CARTESIAN_POINT('',(600.,57.0813206381415,0.));
#2681=CARTESIAN_POINT('',(600.,57.0813206381415,0.));
#2682=CARTESIAN_POINT('',(600.,57.0813206381415,6.35000000000008));
#2683=CARTESIAN_POINT('',(600.,57.0813206381415,6.35000000000008));
#2684=CARTESIAN_POINT('',(600.,57.0813206381415,6.35000000000008));
#2685=CARTESIAN_POINT('Origin',(520.009455205772,57.0813206381415,6.35000000000008));
#2686=CARTESIAN_POINT('',(520.009455205772,57.0813206381415,0.));
#2687=CARTESIAN_POINT('',(520.009455205772,57.0813206381415,0.));
#2688=CARTESIAN_POINT('',(520.009455205772,57.0813206381415,6.35000000000008));
#2689=CARTESIAN_POINT('',(520.009455205772,57.0813206381415,6.35000000000008));
#2690=CARTESIAN_POINT('',(520.009455205772,57.0813206381415,6.35000000000008));
#2691=CARTESIAN_POINT('Origin',(336.61437770265,6.34999999999989,6.35000000000008));
#2692=CARTESIAN_POINT('',(336.61437770265,6.34999999999989,0.));
#2693=CARTESIAN_POINT('',(336.61437770265,6.34999999999989,0.));
#2694=CARTESIAN_POINT('',(336.61437770265,6.34999999999989,6.35000000000008));
#2695=CARTESIAN_POINT('',(336.61437770265,6.34999999999989,6.35000000000008));
#2696=CARTESIAN_POINT('',(336.61437770265,6.34999999999989,6.35000000000008));
#2697=CARTESIAN_POINT('Origin',(261.137671718493,6.34999999999989,6.35000000000008));
#2698=CARTESIAN_POINT('',(261.137671718493,6.34999999999989,0.));
#2699=CARTESIAN_POINT('',(261.137671718493,6.34999999999989,0.));
#2700=CARTESIAN_POINT('',(261.137671718493,6.34999999999989,6.35000000000008));
#2701=CARTESIAN_POINT('',(261.137671718493,6.34999999999989,6.35000000000008));
#2702=CARTESIAN_POINT('',(261.137671718493,6.34999999999989,6.35000000000008));
#2703=CARTESIAN_POINT('Origin',(79.9361966800339,57.1499999999999,6.35000000000008));
#2704=CARTESIAN_POINT('',(79.9361966800339,57.1499999999999,0.));
#2705=CARTESIAN_POINT('',(79.9361966800339,57.1499999999999,0.));
#2706=CARTESIAN_POINT('',(79.9361966800339,57.1499999999999,6.35000000000008));
#2707=CARTESIAN_POINT('',(79.9361966800339,57.1499999999999,6.35000000000008));
#2708=CARTESIAN_POINT('',(79.9361966800339,57.1499999999999,6.35000000000008));
#2709=CARTESIAN_POINT('Origin',(0.,57.1499999999999,6.35000000000008));
#2710=CARTESIAN_POINT('',(0.,57.1499999999999,0.));
#2711=CARTESIAN_POINT('',(0.,57.1499999999999,0.));
#2712=CARTESIAN_POINT('',(0.,57.1499999999999,6.35000000000008));
#2713=CARTESIAN_POINT('',(0.,57.1499999999999,6.35000000000008));
#2714=CARTESIAN_POINT('',(0.,57.1499999999999,6.35000000000008));
#2715=CARTESIAN_POINT('Origin',(0.,0.,6.35000000000008));
#2716=CARTESIAN_POINT('',(0.,0.,0.));
#2717=CARTESIAN_POINT('',(0.,0.,6.35000000000008));
#2718=CARTESIAN_POINT('Origin',(0.,0.,6.35000000000008));
#2719=CARTESIAN_POINT('Origin',(0.,0.,0.));
#2720=CARTESIAN_POINT('',(0.,0.,0.));
#2721=CARTESIAN_POINT('Origin',(0.,0.,6.35));
#2722=CARTESIAN_POINT('',(0.,50.7999999999971,-3.19189119579733E-13));
#2723=CARTESIAN_POINT('',(0.,0.,0.));
#2724=CARTESIAN_POINT('',(0.,0.,0.));
#2725=CARTESIAN_POINT('',(0.,0.,6.35));
#2726=CARTESIAN_POINT('',(0.,0.,6.35));
#2727=CARTESIAN_POINT('',(0.,50.7999999999971,6.35000000000001));
#2728=CARTESIAN_POINT('',(0.,0.,6.35));
#2729=CARTESIAN_POINT('',(0.,50.7999999999971,6.35000000000001));
#2730=CARTESIAN_POINT('Origin',(0.,0.,6.35));
#2731=CARTESIAN_POINT('',(170.,0.,5.20417042793042E-13));
#2732=CARTESIAN_POINT('',(0.,0.,0.));
#2733=CARTESIAN_POINT('',(170.,0.,6.35000000000051));
#2734=CARTESIAN_POINT('',(170.,0.,6.35000000000051));
#2735=CARTESIAN_POINT('',(0.,0.,6.35));
#2736=CARTESIAN_POINT('Origin',(170.,0.,6.35000000000051));
#2737=CARTESIAN_POINT('',(170.,50.7999999999971,4.92661467177413E-13));
#2738=CARTESIAN_POINT('',(170.,0.,5.20417042793042E-13));
#2739=CARTESIAN_POINT('',(170.,50.7999999999971,6.3500000000005));
#2740=CARTESIAN_POINT('',(170.,50.7999999999971,6.3500000000005));
#2741=CARTESIAN_POINT('',(170.,0.,6.35000000000051));
#2742=CARTESIAN_POINT('Origin',(0.,50.7999999999971,6.35000000000001));
#2743=CARTESIAN_POINT('',(0.,50.7999999999971,-3.19189119579733E-13));
#2744=CARTESIAN_POINT('',(0.,50.7999999999971,6.35000000000001));
#2745=CARTESIAN_POINT('Origin',(0.,0.,6.35));
#2746=CARTESIAN_POINT('Origin',(0.,0.,0.));
#2747=CARTESIAN_POINT('',(0.,0.,0.));
#2748=CARTESIAN_POINT('Origin',(0.,0.,0.));
#2749=CARTESIAN_POINT('',(17.6799999999998,5.18791344505844E-14,0.999999999999992));
#2750=CARTESIAN_POINT('Origin',(0.,0.,0.999999999999994));
#2751=CARTESIAN_POINT('',(18.6799999999998,5.63647482807494E-14,-6.00207461602546E-16));
#2752=CARTESIAN_POINT('',(18.6799999999998,5.63647482807494E-14,1.18475909571906E-16));
#2753=CARTESIAN_POINT('Origin',(0.,0.,0.));
#2754=CARTESIAN_POINT('Origin',(0.,0.,54.9999999999998));
#2755=CARTESIAN_POINT('',(17.6799999999998,5.33473634691461E-14,54.9999999999998));
#2756=CARTESIAN_POINT('Origin',(0.,0.,54.9999999999998));
#2757=CARTESIAN_POINT('',(17.6799999999998,5.33473634691461E-14,54.9999999999998));
#2758=CARTESIAN_POINT('Origin',(0.,0.,54.9999999999998));
#2759=CARTESIAN_POINT('',(21.0799999999997,1.44359067849494E-13,0.));
#2760=CARTESIAN_POINT('Origin',(0.,0.,0.));
#2761=CARTESIAN_POINT('',(21.0799999999997,6.36064718285973E-14,54.9999999999998));
#2762=CARTESIAN_POINT('',(21.0799999999997,6.36064718285973E-14,54.9999999999998));
#2763=CARTESIAN_POINT('Origin',(0.,0.,54.9999999999998));
#2764=CARTESIAN_POINT('Origin',(0.,0.,54.9999999999998));
#2765=CARTESIAN_POINT('Origin',(0.,0.,0.));
#2766=CARTESIAN_POINT('',(-393.69551654626,1.3526539764315,500.));
#2767=CARTESIAN_POINT('',(168.20448345374,-30.3973460235685,500.));
#2768=CARTESIAN_POINT('',(168.80448345374,2.62265397643145,550.));
#2769=CARTESIAN_POINT('',(-393.69551654626,-55.7973460235685,493.65));
#2770=CARTESIAN_POINT('',(-39.8955165462598,-55.7973460235685,1474.51299882004));
#2771=CARTESIAN_POINT('',(-355.59551654626,-30.3973460235685,500.));
#2772=CARTESIAN_POINT('',(-393.69551654626,-55.72866666171,1487.3));
#2773=CARTESIAN_POINT('',(-39.8955165462598,-55.7973460235685,1024.51299882004));
#2774=CARTESIAN_POINT('',(-39.8955165462598,-55.7973460235685,574.512998820037));
#2775=CARTESIAN_POINT('',(-317.49551654626,-55.7973460235685,1474.51299882004));
#2776=CARTESIAN_POINT('',(-317.49551654626,-55.7973460235685,1024.51299882004));
#2777=CARTESIAN_POINT('',(-317.49551654626,-55.7973460235685,574.512998820037));
#2778=CARTESIAN_POINT('',(-356.19551654626,2.62265397643144,550.));
#2779=CARTESIAN_POINT('',(168.80448345374,2.62265397643145,1437.3));
#2780=CARTESIAN_POINT('',(-356.19551654626,2.62265397643148,1437.3));
#2781=UNCERTAINTY_MEASURE_WITH_UNIT(LENGTH_MEASURE(0.01),#2795,
'DISTANCE_ACCURACY_VALUE',
'Maximum model space distance between geometric entities at asserted c
onnectivities');
#2782=UNCERTAINTY_MEASURE_WITH_UNIT(LENGTH_MEASURE(0.01),#2795,
'DISTANCE_ACCURACY_VALUE',
'Maximum model space distance between geometric entities at asserted c
onnectivities');
#2783=UNCERTAINTY_MEASURE_WITH_UNIT(LENGTH_MEASURE(0.01),#2795,
'DISTANCE_ACCURACY_VALUE',
'Maximum model space distance between geometric entities at asserted c
onnectivities');
#2784=UNCERTAINTY_MEASURE_WITH_UNIT(LENGTH_MEASURE(0.01),#2795,
'DISTANCE_ACCURACY_VALUE',
'Maximum model space distance between geometric entities at asserted c
onnectivities');
#2785=UNCERTAINTY_MEASURE_WITH_UNIT(LENGTH_MEASURE(0.01),#2795,
'DISTANCE_ACCURACY_VALUE',
'Maximum model space distance between geometric entities at asserted c
onnectivities');
#2786=UNCERTAINTY_MEASURE_WITH_UNIT(LENGTH_MEASURE(0.01),#2795,
'DISTANCE_ACCURACY_VALUE',
'Maximum model space distance between geometric entities at asserted c
onnectivities');
#2787=UNCERTAINTY_MEASURE_WITH_UNIT(LENGTH_MEASURE(0.01),#2795,
'DISTANCE_ACCURACY_VALUE',
'Maximum model space distance between geometric entities at asserted c
onnectivities');
#2788=(
GEOMETRIC_REPRESENTATION_CONTEXT(3)
GLOBAL_UNCERTAINTY_ASSIGNED_CONTEXT((#2781))
GLOBAL_UNIT_ASSIGNED_CONTEXT((#2795,#2797,#2798))
REPRESENTATION_CONTEXT('','3D')
);
#2789=(
GEOMETRIC_REPRESENTATION_CONTEXT(3)
GLOBAL_UNCERTAINTY_ASSIGNED_CONTEXT((#2782))
GLOBAL_UNIT_ASSIGNED_CONTEXT((#2795,#2797,#2798))
REPRESENTATION_CONTEXT('','3D')
);
#2790=(
GEOMETRIC_REPRESENTATION_CONTEXT(3)
GLOBAL_UNCERTAINTY_ASSIGNED_CONTEXT((#2783))
GLOBAL_UNIT_ASSIGNED_CONTEXT((#2795,#2797,#2798))
REPRESENTATION_CONTEXT('','3D')
);
#2791=(
GEOMETRIC_REPRESENTATION_CONTEXT(3)
GLOBAL_UNCERTAINTY_ASSIGNED_CONTEXT((#2784))
GLOBAL_UNIT_ASSIGNED_CONTEXT((#2795,#2797,#2798))
REPRESENTATION_CONTEXT('','3D')
);
#2792=(
GEOMETRIC_REPRESENTATION_CONTEXT(3)
GLOBAL_UNCERTAINTY_ASSIGNED_CONTEXT((#2785))
GLOBAL_UNIT_ASSIGNED_CONTEXT((#2795,#2797,#2798))
REPRESENTATION_CONTEXT('','3D')
);
#2793=(
GEOMETRIC_REPRESENTATION_CONTEXT(3)
GLOBAL_UNCERTAINTY_ASSIGNED_CONTEXT((#2786))
GLOBAL_UNIT_ASSIGNED_CONTEXT((#2795,#2797,#2798))
REPRESENTATION_CONTEXT('','3D')
);
#2794=(
GEOMETRIC_REPRESENTATION_CONTEXT(3)
GLOBAL_UNCERTAINTY_ASSIGNED_CONTEXT((#2787))
GLOBAL_UNIT_ASSIGNED_CONTEXT((#2795,#2797,#2798))
REPRESENTATION_CONTEXT('','3D')
);
#2795=(
LENGTH_UNIT()
NAMED_UNIT(*)
SI_UNIT(.MILLI.,.METRE.)
);
#2796=(
LENGTH_UNIT()
NAMED_UNIT(*)
SI_UNIT($,.METRE.)
);
#2797=(
NAMED_UNIT(*)
PLANE_ANGLE_UNIT()
SI_UNIT($,.RADIAN.)
);
#2798=(
NAMED_UNIT(*)
SI_UNIT($,.STERADIAN.)
SOLID_ANGLE_UNIT()
);
#2799=SHAPE_DEFINITION_REPRESENTATION(#2805,#2826);
#2800=SHAPE_DEFINITION_REPRESENTATION(#2806,#2827);
#2801=SHAPE_DEFINITION_REPRESENTATION(#2807,#2828);
#2802=SHAPE_DEFINITION_REPRESENTATION(#2808,#2829);
#2803=SHAPE_DEFINITION_REPRESENTATION(#2809,#2830);
#2804=SHAPE_DEFINITION_REPRESENTATION(#2810,#2831);
#2805=PRODUCT_DEFINITION_SHAPE('',$,#2833);
#2806=PRODUCT_DEFINITION_SHAPE('',$,#2834);
#2807=PRODUCT_DEFINITION_SHAPE('',$,#2835);
#2808=PRODUCT_DEFINITION_SHAPE('',$,#2836);
#2809=PRODUCT_DEFINITION_SHAPE('',$,#2837);
#2810=PRODUCT_DEFINITION_SHAPE('',$,#2838);
#2811=PRODUCT_DEFINITION_SHAPE($,$,#56);
#2812=PRODUCT_DEFINITION_SHAPE($,$,#57);
#2813=PRODUCT_DEFINITION_SHAPE($,$,#58);
#2814=PRODUCT_DEFINITION_SHAPE($,$,#59);
#2815=PRODUCT_DEFINITION_SHAPE($,$,#60);
#2816=PRODUCT_DEFINITION_SHAPE($,$,#61);
#2817=PRODUCT_DEFINITION_SHAPE($,$,#62);
#2818=PRODUCT_DEFINITION_SHAPE($,$,#63);
#2819=PRODUCT_DEFINITION_SHAPE($,$,#64);
#2820=PRODUCT_DEFINITION_SHAPE($,$,#65);
#2821=PRODUCT_DEFINITION_SHAPE($,$,#66);
#2822=PRODUCT_DEFINITION_SHAPE($,$,#67);
#2823=PRODUCT_DEFINITION_SHAPE($,$,#68);
#2824=PRODUCT_DEFINITION_SHAPE($,$,#69);
#2825=PRODUCT_DEFINITION_SHAPE($,$,#70);
#2826=SHAPE_REPRESENTATION('',(#1702,#1840,#1841,#1842,#1843,#1844,#1845,
#1846,#1847,#1848,#1849,#1850,#1851,#1852,#1853,#1854),#2788);
#2827=SHAPE_REPRESENTATION('',(#1703),#2789);
#2828=SHAPE_REPRESENTATION('',(#1794),#2790);
#2829=SHAPE_REPRESENTATION('',(#1811),#2791);
#2830=SHAPE_REPRESENTATION('',(#1822),#2792);
#2831=SHAPE_REPRESENTATION('',(#1829),#2793);
#2832=PRODUCT_DEFINITION_CONTEXT('part definition',#2852,'design');
#2833=PRODUCT_DEFINITION('MAT-044','MAT-044',#2839,#2832);
#2834=PRODUCT_DEFINITION('Drilled Plate','Drilled Plate',#2840,#2832);
#2835=PRODUCT_DEFINITION('Rectangular Tube','Rectangular Tube',#2841,#2832);
#2836=PRODUCT_DEFINITION('Cover Plate','Cover Plate',#2842,#2832);
#2837=PRODUCT_DEFINITION('Bottom Plate','Bottom Plate',#2843,#2832);
#2838=PRODUCT_DEFINITION('Tube','Tube',#2844,#2832);
#2839=PRODUCT_DEFINITION_FORMATION('',$,#2854);
#2840=PRODUCT_DEFINITION_FORMATION('',$,#2855);
#2841=PRODUCT_DEFINITION_FORMATION('',$,#2856);
#2842=PRODUCT_DEFINITION_FORMATION('',$,#2857);
#2843=PRODUCT_DEFINITION_FORMATION('',$,#2858);
#2844=PRODUCT_DEFINITION_FORMATION('',$,#2859);
#2845=PRODUCT_RELATED_PRODUCT_CATEGORY('MAT-044','MAT-044',(#2854));
#2846=PRODUCT_RELATED_PRODUCT_CATEGORY('Drilled Plate','Drilled Plate',
(#2855));
#2847=PRODUCT_RELATED_PRODUCT_CATEGORY('Rectangular Tube',
'Rectangular Tube',(#2856));
#2848=PRODUCT_RELATED_PRODUCT_CATEGORY('Cover Plate','Cover Plate',(#2857));
#2849=PRODUCT_RELATED_PRODUCT_CATEGORY('Bottom Plate','Bottom Plate',(#2858));
#2850=PRODUCT_RELATED_PRODUCT_CATEGORY('Tube','Tube',(#2859));
#2851=APPLICATION_PROTOCOL_DEFINITION('international standard',
'automotive_design',2009,#2852);
#2852=APPLICATION_CONTEXT(
'Core Data for Automotive Mechanical Design Process');
#2853=PRODUCT_CONTEXT('part definition',#2852,'mechanical');
#2854=PRODUCT('MAT-044','MAT-044','STEP AP214',(#2853));
#2855=PRODUCT('Drilled Plate','Drilled Plate',$,(#2853));
#2856=PRODUCT('Rectangular Tube','Rectangular Tube',$,(#2853));
#2857=PRODUCT('Cover Plate','Cover Plate',$,(#2853));
#2858=PRODUCT('Bottom Plate','Bottom Plate',$,(#2853));
#2859=PRODUCT('Tube','Tube',$,(#2853));
#2860=PRESENTATION_STYLE_ASSIGNMENT((#2864));
#2861=PRESENTATION_STYLE_ASSIGNMENT((#2865));
#2862=PRESENTATION_STYLE_ASSIGNMENT((#2866));
#2863=PRESENTATION_STYLE_ASSIGNMENT((#2867));
#2864=SURFACE_STYLE_USAGE(.BOTH.,#2868);
#2865=SURFACE_STYLE_USAGE(.BOTH.,#2869);
#2866=SURFACE_STYLE_USAGE(.BOTH.,#2870);
#2867=SURFACE_STYLE_USAGE(.BOTH.,#2871);
#2868=SURFACE_SIDE_STYLE('',(#2872));
#2869=SURFACE_SIDE_STYLE('',(#2873));
#2870=SURFACE_SIDE_STYLE('',(#2874));
#2871=SURFACE_SIDE_STYLE('',(#2875));
#2872=SURFACE_STYLE_FILL_AREA(#2876);
#2873=SURFACE_STYLE_FILL_AREA(#2877);
#2874=SURFACE_STYLE_FILL_AREA(#2878);
#2875=SURFACE_STYLE_FILL_AREA(#2879);
#2876=FILL_AREA_STYLE('Steel - Satin',(#2880));
#2877=FILL_AREA_STYLE('Opaque(97,158,199)',(#2881));
#2878=FILL_AREA_STYLE('Opaque(61,176,222)',(#2882));
#2879=FILL_AREA_STYLE('Opaque(227,224,212)',(#2883));
#2880=FILL_AREA_STYLE_COLOUR('Steel - Satin',#2884);
#2881=FILL_AREA_STYLE_COLOUR('Opaque(97,158,199)',#2885);
#2882=FILL_AREA_STYLE_COLOUR('Opaque(61,176,222)',#2886);
#2883=FILL_AREA_STYLE_COLOUR('Opaque(227,224,212)',#2887);
#2884=COLOUR_RGB('Steel - Satin',0.627450980392157,0.627450980392157,0.627450980392157);
#2885=COLOUR_RGB('Opaque(97,158,199)',0.380392156862745,0.619607843137255,
0.780392156862745);
#2886=COLOUR_RGB('Opaque(61,176,222)',0.23921568627451,0.690196078431373,
0.870588235294118);
#2887=COLOUR_RGB('Opaque(227,224,212)',0.890196078431372,0.87843137254902,
0.831372549019608);
ENDSEC;
END-ISO-10303-21;
